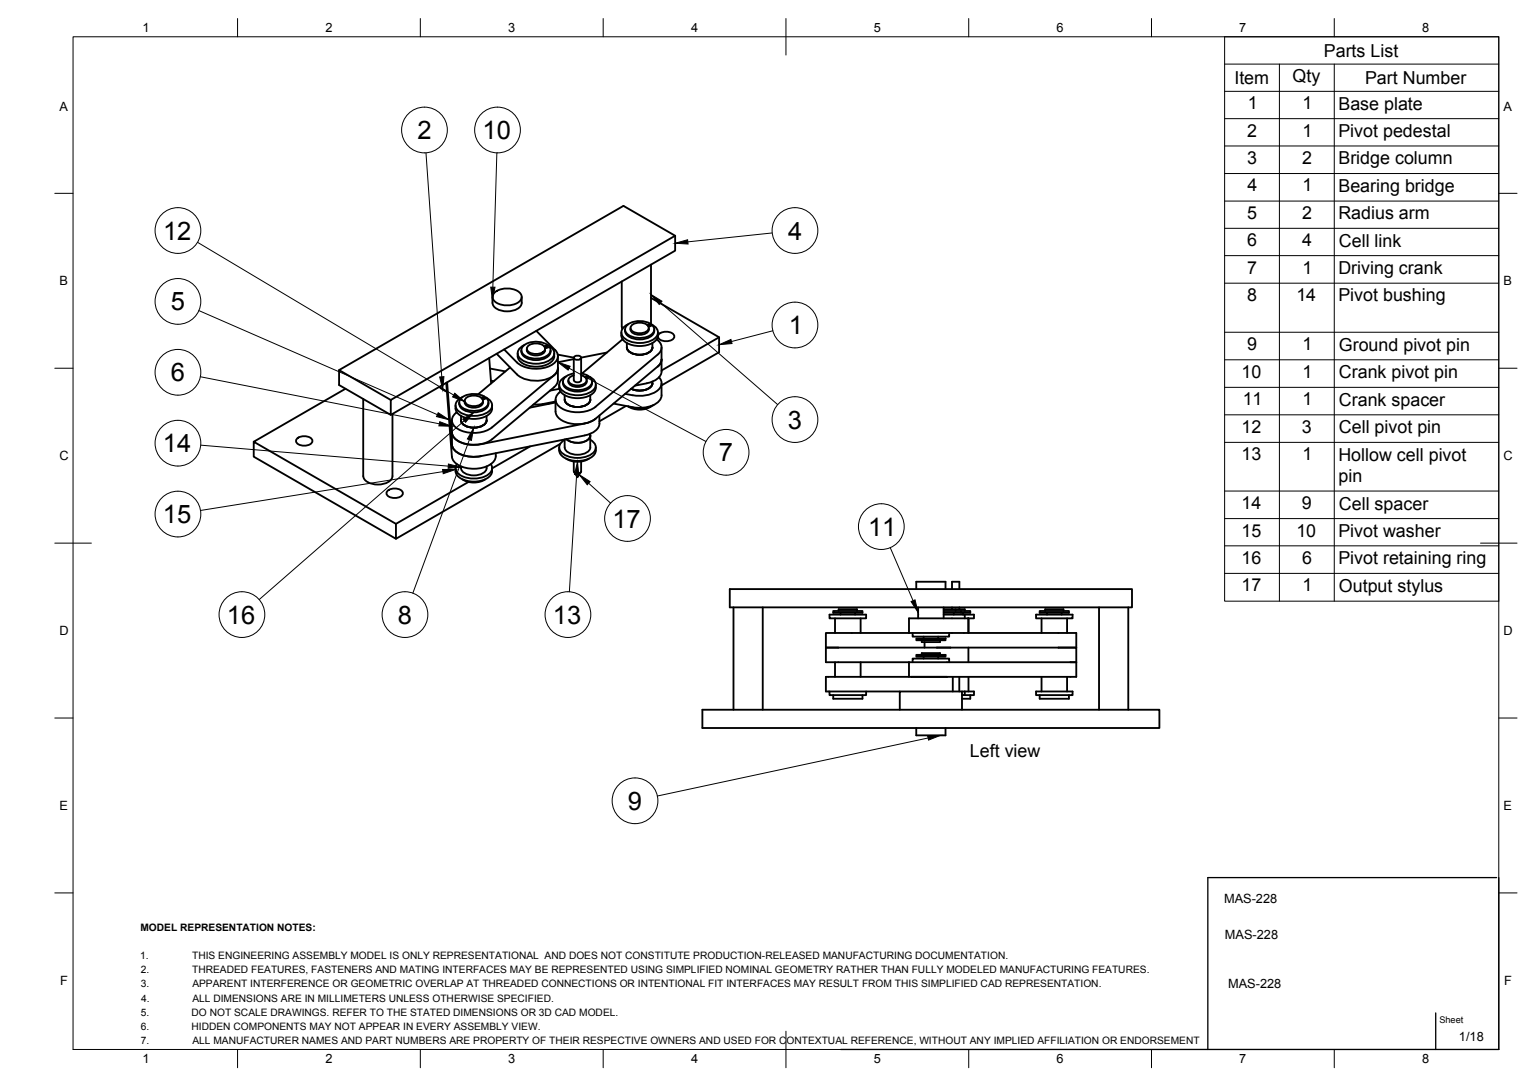
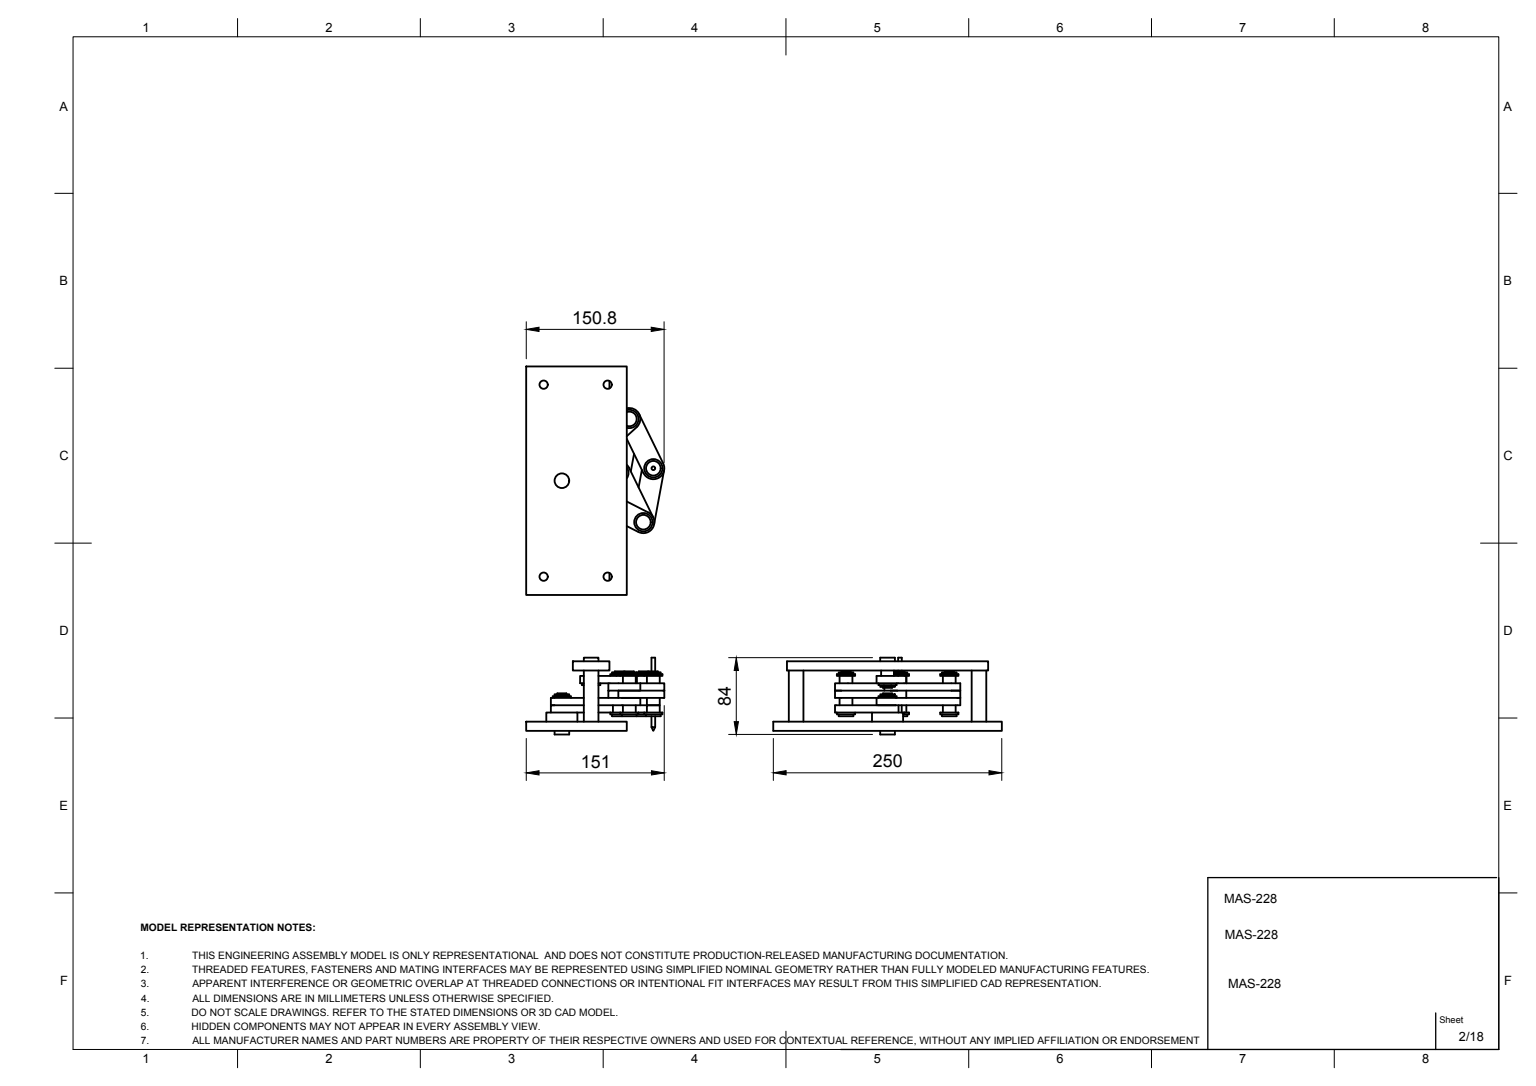
ISO-10303-21;
HEADER;
/* Generated by software containing ST-Developer
 * from STEP Tools, Inc. (www.steptools.com) 
 */

FILE_DESCRIPTION(
/* description */ ('Independent Peaucellier-Lipkin straight-line linkage. Radius arms 100
 mm, inversion-cell links 60 mm, crank radius and fixed-pivot spacing 
32 mm. Inversion constant 6400 mm squared, nominal output straight lin
e X=100 mm. Overhead bearing bridge clears the layered moving links. N
o accuracy or load rating assigned.'),
/* implementation_level */ '2;1');

FILE_NAME(
/* name */ 'MAS-228.step',
/* time_stamp */ '2026-11-09T18:06:16-08:00',
/* author */ (''),
/* organization */ (''),
/* preprocessor_version */ 'ST-DEVELOPER v20.2',
/* originating_system */ 'Autodesk Translation Framework v15.17.0.0',
/* authorisation */ '');

FILE_SCHEMA (('AUTOMOTIVE_DESIGN { 1 0 10303 214 3 1 1 }'));
ENDSEC;

DATA;
#10=MECHANICAL_DESIGN_GEOMETRIC_PRESENTATION_REPRESENTATION('',(#282,#283,
#284,#285,#286,#287,#288,#289,#290,#291,#292,#293,#294,#295,#296,#297,#298),
#3581);
#11=ITEM_DEFINED_TRANSFORMATION($,$,#2074,#2300);
#12=ITEM_DEFINED_TRANSFORMATION($,$,#2096,#2301);
#13=ITEM_DEFINED_TRANSFORMATION($,$,#2132,#2302);
#14=ITEM_DEFINED_TRANSFORMATION($,$,#2105,#2303);
#15=ITEM_DEFINED_TRANSFORMATION($,$,#2138,#2304);
#16=ITEM_DEFINED_TRANSFORMATION($,$,#2155,#2305);
#17=ITEM_DEFINED_TRANSFORMATION($,$,#2115,#2306);
#18=ITEM_DEFINED_TRANSFORMATION($,$,#2238,#2307);
#19=ITEM_DEFINED_TRANSFORMATION($,$,#2132,#2308);
#20=ITEM_DEFINED_TRANSFORMATION($,$,#2138,#2309);
#21=ITEM_DEFINED_TRANSFORMATION($,$,#2155,#2310);
#22=ITEM_DEFINED_TRANSFORMATION($,$,#2155,#2311);
#23=ITEM_DEFINED_TRANSFORMATION($,$,#2155,#2312);
#24=ITEM_DEFINED_TRANSFORMATION($,$,#2172,#2313);
#25=ITEM_DEFINED_TRANSFORMATION($,$,#2190,#2314);
#26=ITEM_DEFINED_TRANSFORMATION($,$,#2208,#2315);
#27=ITEM_DEFINED_TRANSFORMATION($,$,#2253,#2316);
#28=ITEM_DEFINED_TRANSFORMATION($,$,#2217,#2317);
#29=ITEM_DEFINED_TRANSFORMATION($,$,#2271,#2318);
#30=ITEM_DEFINED_TRANSFORMATION($,$,#2280,#2319);
#31=ITEM_DEFINED_TRANSFORMATION($,$,#2238,#2320);
#32=ITEM_DEFINED_TRANSFORMATION($,$,#2238,#2321);
#33=ITEM_DEFINED_TRANSFORMATION($,$,#2238,#2322);
#34=ITEM_DEFINED_TRANSFORMATION($,$,#2238,#2323);
#35=ITEM_DEFINED_TRANSFORMATION($,$,#2238,#2324);
#36=ITEM_DEFINED_TRANSFORMATION($,$,#2238,#2325);
#37=ITEM_DEFINED_TRANSFORMATION($,$,#2238,#2326);
#38=ITEM_DEFINED_TRANSFORMATION($,$,#2238,#2327);
#39=ITEM_DEFINED_TRANSFORMATION($,$,#2238,#2328);
#40=ITEM_DEFINED_TRANSFORMATION($,$,#2238,#2329);
#41=ITEM_DEFINED_TRANSFORMATION($,$,#2238,#2330);
#42=ITEM_DEFINED_TRANSFORMATION($,$,#2238,#2331);
#43=ITEM_DEFINED_TRANSFORMATION($,$,#2238,#2332);
#44=ITEM_DEFINED_TRANSFORMATION($,$,#2289,#2333);
#45=ITEM_DEFINED_TRANSFORMATION($,$,#2247,#2334);
#46=ITEM_DEFINED_TRANSFORMATION($,$,#2280,#2335);
#47=ITEM_DEFINED_TRANSFORMATION($,$,#2289,#2336);
#48=ITEM_DEFINED_TRANSFORMATION($,$,#2271,#2337);
#49=ITEM_DEFINED_TRANSFORMATION($,$,#2280,#2338);
#50=ITEM_DEFINED_TRANSFORMATION($,$,#2280,#2339);
#51=ITEM_DEFINED_TRANSFORMATION($,$,#2289,#2340);
#52=ITEM_DEFINED_TRANSFORMATION($,$,#2253,#2341);
#53=ITEM_DEFINED_TRANSFORMATION($,$,#2271,#2342);
#54=ITEM_DEFINED_TRANSFORMATION($,$,#2271,#2343);
#55=ITEM_DEFINED_TRANSFORMATION($,$,#2280,#2344);
#56=ITEM_DEFINED_TRANSFORMATION($,$,#2280,#2345);
#57=ITEM_DEFINED_TRANSFORMATION($,$,#2289,#2346);
#58=ITEM_DEFINED_TRANSFORMATION($,$,#2253,#2347);
#59=ITEM_DEFINED_TRANSFORMATION($,$,#2271,#2348);
#60=ITEM_DEFINED_TRANSFORMATION($,$,#2271,#2349);
#61=ITEM_DEFINED_TRANSFORMATION($,$,#2280,#2350);
#62=ITEM_DEFINED_TRANSFORMATION($,$,#2280,#2351);
#63=ITEM_DEFINED_TRANSFORMATION($,$,#2289,#2352);
#64=ITEM_DEFINED_TRANSFORMATION($,$,#2271,#2353);
#65=ITEM_DEFINED_TRANSFORMATION($,$,#2271,#2354);
#66=ITEM_DEFINED_TRANSFORMATION($,$,#2271,#2355);
#67=ITEM_DEFINED_TRANSFORMATION($,$,#2280,#2356);
#68=ITEM_DEFINED_TRANSFORMATION($,$,#2280,#2357);
#69=ITEM_DEFINED_TRANSFORMATION($,$,#2289,#2358);
#70=(
REPRESENTATION_RELATIONSHIP($,$,#3682,#3681)
REPRESENTATION_RELATIONSHIP_WITH_TRANSFORMATION(#11)
SHAPE_REPRESENTATION_RELATIONSHIP()
);
#71=(
REPRESENTATION_RELATIONSHIP($,$,#3683,#3681)
REPRESENTATION_RELATIONSHIP_WITH_TRANSFORMATION(#12)
SHAPE_REPRESENTATION_RELATIONSHIP()
);
#72=(
REPRESENTATION_RELATIONSHIP($,$,#3686,#3681)
REPRESENTATION_RELATIONSHIP_WITH_TRANSFORMATION(#13)
SHAPE_REPRESENTATION_RELATIONSHIP()
);
#73=(
REPRESENTATION_RELATIONSHIP($,$,#3684,#3681)
REPRESENTATION_RELATIONSHIP_WITH_TRANSFORMATION(#14)
SHAPE_REPRESENTATION_RELATIONSHIP()
);
#74=(
REPRESENTATION_RELATIONSHIP($,$,#3687,#3681)
REPRESENTATION_RELATIONSHIP_WITH_TRANSFORMATION(#15)
SHAPE_REPRESENTATION_RELATIONSHIP()
);
#75=(
REPRESENTATION_RELATIONSHIP($,$,#3688,#3681)
REPRESENTATION_RELATIONSHIP_WITH_TRANSFORMATION(#16)
SHAPE_REPRESENTATION_RELATIONSHIP()
);
#76=(
REPRESENTATION_RELATIONSHIP($,$,#3685,#3681)
REPRESENTATION_RELATIONSHIP_WITH_TRANSFORMATION(#17)
SHAPE_REPRESENTATION_RELATIONSHIP()
);
#77=(
REPRESENTATION_RELATIONSHIP($,$,#3693,#3681)
REPRESENTATION_RELATIONSHIP_WITH_TRANSFORMATION(#18)
SHAPE_REPRESENTATION_RELATIONSHIP()
);
#78=(
REPRESENTATION_RELATIONSHIP($,$,#3686,#3681)
REPRESENTATION_RELATIONSHIP_WITH_TRANSFORMATION(#19)
SHAPE_REPRESENTATION_RELATIONSHIP()
);
#79=(
REPRESENTATION_RELATIONSHIP($,$,#3687,#3681)
REPRESENTATION_RELATIONSHIP_WITH_TRANSFORMATION(#20)
SHAPE_REPRESENTATION_RELATIONSHIP()
);
#80=(
REPRESENTATION_RELATIONSHIP($,$,#3688,#3681)
REPRESENTATION_RELATIONSHIP_WITH_TRANSFORMATION(#21)
SHAPE_REPRESENTATION_RELATIONSHIP()
);
#81=(
REPRESENTATION_RELATIONSHIP($,$,#3688,#3681)
REPRESENTATION_RELATIONSHIP_WITH_TRANSFORMATION(#22)
SHAPE_REPRESENTATION_RELATIONSHIP()
);
#82=(
REPRESENTATION_RELATIONSHIP($,$,#3688,#3681)
REPRESENTATION_RELATIONSHIP_WITH_TRANSFORMATION(#23)
SHAPE_REPRESENTATION_RELATIONSHIP()
);
#83=(
REPRESENTATION_RELATIONSHIP($,$,#3689,#3681)
REPRESENTATION_RELATIONSHIP_WITH_TRANSFORMATION(#24)
SHAPE_REPRESENTATION_RELATIONSHIP()
);
#84=(
REPRESENTATION_RELATIONSHIP($,$,#3690,#3681)
REPRESENTATION_RELATIONSHIP_WITH_TRANSFORMATION(#25)
SHAPE_REPRESENTATION_RELATIONSHIP()
);
#85=(
REPRESENTATION_RELATIONSHIP($,$,#3691,#3681)
REPRESENTATION_RELATIONSHIP_WITH_TRANSFORMATION(#26)
SHAPE_REPRESENTATION_RELATIONSHIP()
);
#86=(
REPRESENTATION_RELATIONSHIP($,$,#3695,#3681)
REPRESENTATION_RELATIONSHIP_WITH_TRANSFORMATION(#27)
SHAPE_REPRESENTATION_RELATIONSHIP()
);
#87=(
REPRESENTATION_RELATIONSHIP($,$,#3692,#3681)
REPRESENTATION_RELATIONSHIP_WITH_TRANSFORMATION(#28)
SHAPE_REPRESENTATION_RELATIONSHIP()
);
#88=(
REPRESENTATION_RELATIONSHIP($,$,#3696,#3681)
REPRESENTATION_RELATIONSHIP_WITH_TRANSFORMATION(#29)
SHAPE_REPRESENTATION_RELATIONSHIP()
);
#89=(
REPRESENTATION_RELATIONSHIP($,$,#3697,#3681)
REPRESENTATION_RELATIONSHIP_WITH_TRANSFORMATION(#30)
SHAPE_REPRESENTATION_RELATIONSHIP()
);
#90=(
REPRESENTATION_RELATIONSHIP($,$,#3693,#3681)
REPRESENTATION_RELATIONSHIP_WITH_TRANSFORMATION(#31)
SHAPE_REPRESENTATION_RELATIONSHIP()
);
#91=(
REPRESENTATION_RELATIONSHIP($,$,#3693,#3681)
REPRESENTATION_RELATIONSHIP_WITH_TRANSFORMATION(#32)
SHAPE_REPRESENTATION_RELATIONSHIP()
);
#92=(
REPRESENTATION_RELATIONSHIP($,$,#3693,#3681)
REPRESENTATION_RELATIONSHIP_WITH_TRANSFORMATION(#33)
SHAPE_REPRESENTATION_RELATIONSHIP()
);
#93=(
REPRESENTATION_RELATIONSHIP($,$,#3693,#3681)
REPRESENTATION_RELATIONSHIP_WITH_TRANSFORMATION(#34)
SHAPE_REPRESENTATION_RELATIONSHIP()
);
#94=(
REPRESENTATION_RELATIONSHIP($,$,#3693,#3681)
REPRESENTATION_RELATIONSHIP_WITH_TRANSFORMATION(#35)
SHAPE_REPRESENTATION_RELATIONSHIP()
);
#95=(
REPRESENTATION_RELATIONSHIP($,$,#3693,#3681)
REPRESENTATION_RELATIONSHIP_WITH_TRANSFORMATION(#36)
SHAPE_REPRESENTATION_RELATIONSHIP()
);
#96=(
REPRESENTATION_RELATIONSHIP($,$,#3693,#3681)
REPRESENTATION_RELATIONSHIP_WITH_TRANSFORMATION(#37)
SHAPE_REPRESENTATION_RELATIONSHIP()
);
#97=(
REPRESENTATION_RELATIONSHIP($,$,#3693,#3681)
REPRESENTATION_RELATIONSHIP_WITH_TRANSFORMATION(#38)
SHAPE_REPRESENTATION_RELATIONSHIP()
);
#98=(
REPRESENTATION_RELATIONSHIP($,$,#3693,#3681)
REPRESENTATION_RELATIONSHIP_WITH_TRANSFORMATION(#39)
SHAPE_REPRESENTATION_RELATIONSHIP()
);
#99=(
REPRESENTATION_RELATIONSHIP($,$,#3693,#3681)
REPRESENTATION_RELATIONSHIP_WITH_TRANSFORMATION(#40)
SHAPE_REPRESENTATION_RELATIONSHIP()
);
#100=(
REPRESENTATION_RELATIONSHIP($,$,#3693,#3681)
REPRESENTATION_RELATIONSHIP_WITH_TRANSFORMATION(#41)
SHAPE_REPRESENTATION_RELATIONSHIP()
);
#101=(
REPRESENTATION_RELATIONSHIP($,$,#3693,#3681)
REPRESENTATION_RELATIONSHIP_WITH_TRANSFORMATION(#42)
SHAPE_REPRESENTATION_RELATIONSHIP()
);
#102=(
REPRESENTATION_RELATIONSHIP($,$,#3693,#3681)
REPRESENTATION_RELATIONSHIP_WITH_TRANSFORMATION(#43)
SHAPE_REPRESENTATION_RELATIONSHIP()
);
#103=(
REPRESENTATION_RELATIONSHIP($,$,#3698,#3681)
REPRESENTATION_RELATIONSHIP_WITH_TRANSFORMATION(#44)
SHAPE_REPRESENTATION_RELATIONSHIP()
);
#104=(
REPRESENTATION_RELATIONSHIP($,$,#3694,#3681)
REPRESENTATION_RELATIONSHIP_WITH_TRANSFORMATION(#45)
SHAPE_REPRESENTATION_RELATIONSHIP()
);
#105=(
REPRESENTATION_RELATIONSHIP($,$,#3697,#3681)
REPRESENTATION_RELATIONSHIP_WITH_TRANSFORMATION(#46)
SHAPE_REPRESENTATION_RELATIONSHIP()
);
#106=(
REPRESENTATION_RELATIONSHIP($,$,#3698,#3681)
REPRESENTATION_RELATIONSHIP_WITH_TRANSFORMATION(#47)
SHAPE_REPRESENTATION_RELATIONSHIP()
);
#107=(
REPRESENTATION_RELATIONSHIP($,$,#3696,#3681)
REPRESENTATION_RELATIONSHIP_WITH_TRANSFORMATION(#48)
SHAPE_REPRESENTATION_RELATIONSHIP()
);
#108=(
REPRESENTATION_RELATIONSHIP($,$,#3697,#3681)
REPRESENTATION_RELATIONSHIP_WITH_TRANSFORMATION(#49)
SHAPE_REPRESENTATION_RELATIONSHIP()
);
#109=(
REPRESENTATION_RELATIONSHIP($,$,#3697,#3681)
REPRESENTATION_RELATIONSHIP_WITH_TRANSFORMATION(#50)
SHAPE_REPRESENTATION_RELATIONSHIP()
);
#110=(
REPRESENTATION_RELATIONSHIP($,$,#3698,#3681)
REPRESENTATION_RELATIONSHIP_WITH_TRANSFORMATION(#51)
SHAPE_REPRESENTATION_RELATIONSHIP()
);
#111=(
REPRESENTATION_RELATIONSHIP($,$,#3695,#3681)
REPRESENTATION_RELATIONSHIP_WITH_TRANSFORMATION(#52)
SHAPE_REPRESENTATION_RELATIONSHIP()
);
#112=(
REPRESENTATION_RELATIONSHIP($,$,#3696,#3681)
REPRESENTATION_RELATIONSHIP_WITH_TRANSFORMATION(#53)
SHAPE_REPRESENTATION_RELATIONSHIP()
);
#113=(
REPRESENTATION_RELATIONSHIP($,$,#3696,#3681)
REPRESENTATION_RELATIONSHIP_WITH_TRANSFORMATION(#54)
SHAPE_REPRESENTATION_RELATIONSHIP()
);
#114=(
REPRESENTATION_RELATIONSHIP($,$,#3697,#3681)
REPRESENTATION_RELATIONSHIP_WITH_TRANSFORMATION(#55)
SHAPE_REPRESENTATION_RELATIONSHIP()
);
#115=(
REPRESENTATION_RELATIONSHIP($,$,#3697,#3681)
REPRESENTATION_RELATIONSHIP_WITH_TRANSFORMATION(#56)
SHAPE_REPRESENTATION_RELATIONSHIP()
);
#116=(
REPRESENTATION_RELATIONSHIP($,$,#3698,#3681)
REPRESENTATION_RELATIONSHIP_WITH_TRANSFORMATION(#57)
SHAPE_REPRESENTATION_RELATIONSHIP()
);
#117=(
REPRESENTATION_RELATIONSHIP($,$,#3695,#3681)
REPRESENTATION_RELATIONSHIP_WITH_TRANSFORMATION(#58)
SHAPE_REPRESENTATION_RELATIONSHIP()
);
#118=(
REPRESENTATION_RELATIONSHIP($,$,#3696,#3681)
REPRESENTATION_RELATIONSHIP_WITH_TRANSFORMATION(#59)
SHAPE_REPRESENTATION_RELATIONSHIP()
);
#119=(
REPRESENTATION_RELATIONSHIP($,$,#3696,#3681)
REPRESENTATION_RELATIONSHIP_WITH_TRANSFORMATION(#60)
SHAPE_REPRESENTATION_RELATIONSHIP()
);
#120=(
REPRESENTATION_RELATIONSHIP($,$,#3697,#3681)
REPRESENTATION_RELATIONSHIP_WITH_TRANSFORMATION(#61)
SHAPE_REPRESENTATION_RELATIONSHIP()
);
#121=(
REPRESENTATION_RELATIONSHIP($,$,#3697,#3681)
REPRESENTATION_RELATIONSHIP_WITH_TRANSFORMATION(#62)
SHAPE_REPRESENTATION_RELATIONSHIP()
);
#122=(
REPRESENTATION_RELATIONSHIP($,$,#3698,#3681)
REPRESENTATION_RELATIONSHIP_WITH_TRANSFORMATION(#63)
SHAPE_REPRESENTATION_RELATIONSHIP()
);
#123=(
REPRESENTATION_RELATIONSHIP($,$,#3696,#3681)
REPRESENTATION_RELATIONSHIP_WITH_TRANSFORMATION(#64)
SHAPE_REPRESENTATION_RELATIONSHIP()
);
#124=(
REPRESENTATION_RELATIONSHIP($,$,#3696,#3681)
REPRESENTATION_RELATIONSHIP_WITH_TRANSFORMATION(#65)
SHAPE_REPRESENTATION_RELATIONSHIP()
);
#125=(
REPRESENTATION_RELATIONSHIP($,$,#3696,#3681)
REPRESENTATION_RELATIONSHIP_WITH_TRANSFORMATION(#66)
SHAPE_REPRESENTATION_RELATIONSHIP()
);
#126=(
REPRESENTATION_RELATIONSHIP($,$,#3697,#3681)
REPRESENTATION_RELATIONSHIP_WITH_TRANSFORMATION(#67)
SHAPE_REPRESENTATION_RELATIONSHIP()
);
#127=(
REPRESENTATION_RELATIONSHIP($,$,#3697,#3681)
REPRESENTATION_RELATIONSHIP_WITH_TRANSFORMATION(#68)
SHAPE_REPRESENTATION_RELATIONSHIP()
);
#128=(
REPRESENTATION_RELATIONSHIP($,$,#3698,#3681)
REPRESENTATION_RELATIONSHIP_WITH_TRANSFORMATION(#69)
SHAPE_REPRESENTATION_RELATIONSHIP()
);
#129=CONTEXT_DEPENDENT_SHAPE_REPRESENTATION(#70,#3622);
#130=CONTEXT_DEPENDENT_SHAPE_REPRESENTATION(#71,#3623);
#131=CONTEXT_DEPENDENT_SHAPE_REPRESENTATION(#72,#3624);
#132=CONTEXT_DEPENDENT_SHAPE_REPRESENTATION(#73,#3625);
#133=CONTEXT_DEPENDENT_SHAPE_REPRESENTATION(#74,#3626);
#134=CONTEXT_DEPENDENT_SHAPE_REPRESENTATION(#75,#3627);
#135=CONTEXT_DEPENDENT_SHAPE_REPRESENTATION(#76,#3628);
#136=CONTEXT_DEPENDENT_SHAPE_REPRESENTATION(#77,#3629);
#137=CONTEXT_DEPENDENT_SHAPE_REPRESENTATION(#78,#3630);
#138=CONTEXT_DEPENDENT_SHAPE_REPRESENTATION(#79,#3631);
#139=CONTEXT_DEPENDENT_SHAPE_REPRESENTATION(#80,#3632);
#140=CONTEXT_DEPENDENT_SHAPE_REPRESENTATION(#81,#3633);
#141=CONTEXT_DEPENDENT_SHAPE_REPRESENTATION(#82,#3634);
#142=CONTEXT_DEPENDENT_SHAPE_REPRESENTATION(#83,#3635);
#143=CONTEXT_DEPENDENT_SHAPE_REPRESENTATION(#84,#3636);
#144=CONTEXT_DEPENDENT_SHAPE_REPRESENTATION(#85,#3637);
#145=CONTEXT_DEPENDENT_SHAPE_REPRESENTATION(#86,#3638);
#146=CONTEXT_DEPENDENT_SHAPE_REPRESENTATION(#87,#3639);
#147=CONTEXT_DEPENDENT_SHAPE_REPRESENTATION(#88,#3640);
#148=CONTEXT_DEPENDENT_SHAPE_REPRESENTATION(#89,#3641);
#149=CONTEXT_DEPENDENT_SHAPE_REPRESENTATION(#90,#3642);
#150=CONTEXT_DEPENDENT_SHAPE_REPRESENTATION(#91,#3643);
#151=CONTEXT_DEPENDENT_SHAPE_REPRESENTATION(#92,#3644);
#152=CONTEXT_DEPENDENT_SHAPE_REPRESENTATION(#93,#3645);
#153=CONTEXT_DEPENDENT_SHAPE_REPRESENTATION(#94,#3646);
#154=CONTEXT_DEPENDENT_SHAPE_REPRESENTATION(#95,#3647);
#155=CONTEXT_DEPENDENT_SHAPE_REPRESENTATION(#96,#3648);
#156=CONTEXT_DEPENDENT_SHAPE_REPRESENTATION(#97,#3649);
#157=CONTEXT_DEPENDENT_SHAPE_REPRESENTATION(#98,#3650);
#158=CONTEXT_DEPENDENT_SHAPE_REPRESENTATION(#99,#3651);
#159=CONTEXT_DEPENDENT_SHAPE_REPRESENTATION(#100,#3652);
#160=CONTEXT_DEPENDENT_SHAPE_REPRESENTATION(#101,#3653);
#161=CONTEXT_DEPENDENT_SHAPE_REPRESENTATION(#102,#3654);
#162=CONTEXT_DEPENDENT_SHAPE_REPRESENTATION(#103,#3655);
#163=CONTEXT_DEPENDENT_SHAPE_REPRESENTATION(#104,#3656);
#164=CONTEXT_DEPENDENT_SHAPE_REPRESENTATION(#105,#3657);
#165=CONTEXT_DEPENDENT_SHAPE_REPRESENTATION(#106,#3658);
#166=CONTEXT_DEPENDENT_SHAPE_REPRESENTATION(#107,#3659);
#167=CONTEXT_DEPENDENT_SHAPE_REPRESENTATION(#108,#3660);
#168=CONTEXT_DEPENDENT_SHAPE_REPRESENTATION(#109,#3661);
#169=CONTEXT_DEPENDENT_SHAPE_REPRESENTATION(#110,#3662);
#170=CONTEXT_DEPENDENT_SHAPE_REPRESENTATION(#111,#3663);
#171=CONTEXT_DEPENDENT_SHAPE_REPRESENTATION(#112,#3664);
#172=CONTEXT_DEPENDENT_SHAPE_REPRESENTATION(#113,#3665);
#173=CONTEXT_DEPENDENT_SHAPE_REPRESENTATION(#114,#3666);
#174=CONTEXT_DEPENDENT_SHAPE_REPRESENTATION(#115,#3667);
#175=CONTEXT_DEPENDENT_SHAPE_REPRESENTATION(#116,#3668);
#176=CONTEXT_DEPENDENT_SHAPE_REPRESENTATION(#117,#3669);
#177=CONTEXT_DEPENDENT_SHAPE_REPRESENTATION(#118,#3670);
#178=CONTEXT_DEPENDENT_SHAPE_REPRESENTATION(#119,#3671);
#179=CONTEXT_DEPENDENT_SHAPE_REPRESENTATION(#120,#3672);
#180=CONTEXT_DEPENDENT_SHAPE_REPRESENTATION(#121,#3673);
#181=CONTEXT_DEPENDENT_SHAPE_REPRESENTATION(#122,#3674);
#182=CONTEXT_DEPENDENT_SHAPE_REPRESENTATION(#123,#3675);
#183=CONTEXT_DEPENDENT_SHAPE_REPRESENTATION(#124,#3676);
#184=CONTEXT_DEPENDENT_SHAPE_REPRESENTATION(#125,#3677);
#185=CONTEXT_DEPENDENT_SHAPE_REPRESENTATION(#126,#3678);
#186=CONTEXT_DEPENDENT_SHAPE_REPRESENTATION(#127,#3679);
#187=CONTEXT_DEPENDENT_SHAPE_REPRESENTATION(#128,#3680);
#188=NEXT_ASSEMBLY_USAGE_OCCURRENCE('Base plate:1','Base plate:1',
'Base plate:1',#3700,#3701,'Base plate:1');
#189=NEXT_ASSEMBLY_USAGE_OCCURRENCE('Pivot pedestal:1',
'Pivot pedestal:1','Pivot pedestal:1',#3700,#3702,'Pivot pedestal:1');
#190=NEXT_ASSEMBLY_USAGE_OCCURRENCE('Bridge column:1','Bridge column:1',
'Bridge column:1',#3700,#3705,'Bridge column:1');
#191=NEXT_ASSEMBLY_USAGE_OCCURRENCE('Bearing bridge:1',
'Bearing bridge:1','Bearing bridge:1',#3700,#3703,'Bearing bridge:1');
#192=NEXT_ASSEMBLY_USAGE_OCCURRENCE('Radius arm:1','Radius arm:1',
'Radius arm:1',#3700,#3706,'Radius arm:1');
#193=NEXT_ASSEMBLY_USAGE_OCCURRENCE('Cell link:1','Cell link:1',
'Cell link:1',#3700,#3707,'Cell link:1');
#194=NEXT_ASSEMBLY_USAGE_OCCURRENCE('Driving crank:1','Driving crank:1',
'Driving crank:1',#3700,#3704,'Driving crank:1');
#195=NEXT_ASSEMBLY_USAGE_OCCURRENCE('Pivot bushing:1','Pivot bushing:1',
'Pivot bushing:1',#3700,#3712,'Pivot bushing:1');
#196=NEXT_ASSEMBLY_USAGE_OCCURRENCE('Bridge column:2','Bridge column:2',
'Bridge column:2',#3700,#3705,'Bridge column:2');
#197=NEXT_ASSEMBLY_USAGE_OCCURRENCE('Radius arm:2','Radius arm:2',
'Radius arm:2',#3700,#3706,'Radius arm:2');
#198=NEXT_ASSEMBLY_USAGE_OCCURRENCE('Cell link:2','Cell link:2',
'Cell link:2',#3700,#3707,'Cell link:2');
#199=NEXT_ASSEMBLY_USAGE_OCCURRENCE('Cell link:3','Cell link:3',
'Cell link:3',#3700,#3707,'Cell link:3');
#200=NEXT_ASSEMBLY_USAGE_OCCURRENCE('Cell link:4','Cell link:4',
'Cell link:4',#3700,#3707,'Cell link:4');
#201=NEXT_ASSEMBLY_USAGE_OCCURRENCE('Ground pivot pin:1',
'Ground pivot pin:1','Ground pivot pin:1',#3700,#3708,
'Ground pivot pin:1');
#202=NEXT_ASSEMBLY_USAGE_OCCURRENCE('Crank pivot pin:1',
'Crank pivot pin:1','Crank pivot pin:1',#3700,#3709,'Crank pivot pin:1');
#203=NEXT_ASSEMBLY_USAGE_OCCURRENCE('Crank spacer:1','Crank spacer:1',
'Crank spacer:1',#3700,#3710,'Crank spacer:1');
#204=NEXT_ASSEMBLY_USAGE_OCCURRENCE('Cell pivot pin:1',
'Cell pivot pin:1','Cell pivot pin:1',#3700,#3714,'Cell pivot pin:1');
#205=NEXT_ASSEMBLY_USAGE_OCCURRENCE('Hollow cell pivot pin:1',
'Hollow cell pivot pin:1','Hollow cell pivot pin:1',#3700,#3711,
'Hollow cell pivot pin:1');
#206=NEXT_ASSEMBLY_USAGE_OCCURRENCE('Cell spacer:1','Cell spacer:1',
'Cell spacer:1',#3700,#3715,'Cell spacer:1');
#207=NEXT_ASSEMBLY_USAGE_OCCURRENCE('Pivot washer:1','Pivot washer:1',
'Pivot washer:1',#3700,#3716,'Pivot washer:1');
#208=NEXT_ASSEMBLY_USAGE_OCCURRENCE('Pivot bushing:2','Pivot bushing:2',
'Pivot bushing:2',#3700,#3712,'Pivot bushing:2');
#209=NEXT_ASSEMBLY_USAGE_OCCURRENCE('Pivot bushing:3','Pivot bushing:3',
'Pivot bushing:3',#3700,#3712,'Pivot bushing:3');
#210=NEXT_ASSEMBLY_USAGE_OCCURRENCE('Pivot bushing:4','Pivot bushing:4',
'Pivot bushing:4',#3700,#3712,'Pivot bushing:4');
#211=NEXT_ASSEMBLY_USAGE_OCCURRENCE('Pivot bushing:5','Pivot bushing:5',
'Pivot bushing:5',#3700,#3712,'Pivot bushing:5');
#212=NEXT_ASSEMBLY_USAGE_OCCURRENCE('Pivot bushing:6','Pivot bushing:6',
'Pivot bushing:6',#3700,#3712,'Pivot bushing:6');
#213=NEXT_ASSEMBLY_USAGE_OCCURRENCE('Pivot bushing:7','Pivot bushing:7',
'Pivot bushing:7',#3700,#3712,'Pivot bushing:7');
#214=NEXT_ASSEMBLY_USAGE_OCCURRENCE('Pivot bushing:8','Pivot bushing:8',
'Pivot bushing:8',#3700,#3712,'Pivot bushing:8');
#215=NEXT_ASSEMBLY_USAGE_OCCURRENCE('Pivot bushing:9','Pivot bushing:9',
'Pivot bushing:9',#3700,#3712,'Pivot bushing:9');
#216=NEXT_ASSEMBLY_USAGE_OCCURRENCE('Pivot bushing:10',
'Pivot bushing:10','Pivot bushing:10',#3700,#3712,'Pivot bushing:10');
#217=NEXT_ASSEMBLY_USAGE_OCCURRENCE('Pivot bushing:11',
'Pivot bushing:11','Pivot bushing:11',#3700,#3712,'Pivot bushing:11');
#218=NEXT_ASSEMBLY_USAGE_OCCURRENCE('Pivot bushing:12',
'Pivot bushing:12','Pivot bushing:12',#3700,#3712,'Pivot bushing:12');
#219=NEXT_ASSEMBLY_USAGE_OCCURRENCE('Pivot bushing:13',
'Pivot bushing:13','Pivot bushing:13',#3700,#3712,'Pivot bushing:13');
#220=NEXT_ASSEMBLY_USAGE_OCCURRENCE('Pivot bushing:14',
'Pivot bushing:14','Pivot bushing:14',#3700,#3712,'Pivot bushing:14');
#221=NEXT_ASSEMBLY_USAGE_OCCURRENCE('Pivot retaining ring:1',
'Pivot retaining ring:1','Pivot retaining ring:1',#3700,#3717,
'Pivot retaining ring:1');
#222=NEXT_ASSEMBLY_USAGE_OCCURRENCE('Output stylus:1','Output stylus:1',
'Output stylus:1',#3700,#3713,'Output stylus:1');
#223=NEXT_ASSEMBLY_USAGE_OCCURRENCE('Pivot washer:2','Pivot washer:2',
'Pivot washer:2',#3700,#3716,'Pivot washer:2');
#224=NEXT_ASSEMBLY_USAGE_OCCURRENCE('Pivot retaining ring:2',
'Pivot retaining ring:2','Pivot retaining ring:2',#3700,#3717,
'Pivot retaining ring:2');
#225=NEXT_ASSEMBLY_USAGE_OCCURRENCE('Cell spacer:2','Cell spacer:2',
'Cell spacer:2',#3700,#3715,'Cell spacer:2');
#226=NEXT_ASSEMBLY_USAGE_OCCURRENCE('Pivot washer:3','Pivot washer:3',
'Pivot washer:3',#3700,#3716,'Pivot washer:3');
#227=NEXT_ASSEMBLY_USAGE_OCCURRENCE('Pivot washer:4','Pivot washer:4',
'Pivot washer:4',#3700,#3716,'Pivot washer:4');
#228=NEXT_ASSEMBLY_USAGE_OCCURRENCE('Pivot retaining ring:3',
'Pivot retaining ring:3','Pivot retaining ring:3',#3700,#3717,
'Pivot retaining ring:3');
#229=NEXT_ASSEMBLY_USAGE_OCCURRENCE('Cell pivot pin:2',
'Cell pivot pin:2','Cell pivot pin:2',#3700,#3714,'Cell pivot pin:2');
#230=NEXT_ASSEMBLY_USAGE_OCCURRENCE('Cell spacer:3','Cell spacer:3',
'Cell spacer:3',#3700,#3715,'Cell spacer:3');
#231=NEXT_ASSEMBLY_USAGE_OCCURRENCE('Cell spacer:4','Cell spacer:4',
'Cell spacer:4',#3700,#3715,'Cell spacer:4');
#232=NEXT_ASSEMBLY_USAGE_OCCURRENCE('Pivot washer:5','Pivot washer:5',
'Pivot washer:5',#3700,#3716,'Pivot washer:5');
#233=NEXT_ASSEMBLY_USAGE_OCCURRENCE('Pivot washer:6','Pivot washer:6',
'Pivot washer:6',#3700,#3716,'Pivot washer:6');
#234=NEXT_ASSEMBLY_USAGE_OCCURRENCE('Pivot retaining ring:4',
'Pivot retaining ring:4','Pivot retaining ring:4',#3700,#3717,
'Pivot retaining ring:4');
#235=NEXT_ASSEMBLY_USAGE_OCCURRENCE('Cell pivot pin:3',
'Cell pivot pin:3','Cell pivot pin:3',#3700,#3714,'Cell pivot pin:3');
#236=NEXT_ASSEMBLY_USAGE_OCCURRENCE('Cell spacer:5','Cell spacer:5',
'Cell spacer:5',#3700,#3715,'Cell spacer:5');
#237=NEXT_ASSEMBLY_USAGE_OCCURRENCE('Cell spacer:6','Cell spacer:6',
'Cell spacer:6',#3700,#3715,'Cell spacer:6');
#238=NEXT_ASSEMBLY_USAGE_OCCURRENCE('Pivot washer:7','Pivot washer:7',
'Pivot washer:7',#3700,#3716,'Pivot washer:7');
#239=NEXT_ASSEMBLY_USAGE_OCCURRENCE('Pivot washer:8','Pivot washer:8',
'Pivot washer:8',#3700,#3716,'Pivot washer:8');
#240=NEXT_ASSEMBLY_USAGE_OCCURRENCE('Pivot retaining ring:5',
'Pivot retaining ring:5','Pivot retaining ring:5',#3700,#3717,
'Pivot retaining ring:5');
#241=NEXT_ASSEMBLY_USAGE_OCCURRENCE('Cell spacer:7','Cell spacer:7',
'Cell spacer:7',#3700,#3715,'Cell spacer:7');
#242=NEXT_ASSEMBLY_USAGE_OCCURRENCE('Cell spacer:8','Cell spacer:8',
'Cell spacer:8',#3700,#3715,'Cell spacer:8');
#243=NEXT_ASSEMBLY_USAGE_OCCURRENCE('Cell spacer:9','Cell spacer:9',
'Cell spacer:9',#3700,#3715,'Cell spacer:9');
#244=NEXT_ASSEMBLY_USAGE_OCCURRENCE('Pivot washer:9','Pivot washer:9',
'Pivot washer:9',#3700,#3716,'Pivot washer:9');
#245=NEXT_ASSEMBLY_USAGE_OCCURRENCE('Pivot washer:10','Pivot washer:10',
'Pivot washer:10',#3700,#3716,'Pivot washer:10');
#246=NEXT_ASSEMBLY_USAGE_OCCURRENCE('Pivot retaining ring:6',
'Pivot retaining ring:6','Pivot retaining ring:6',#3700,#3717,
'Pivot retaining ring:6');
#247=CONICAL_SURFACE('',#2252,1.,0.463647609000806);
#248=SHAPE_REPRESENTATION_RELATIONSHIP('SRR','None',#3682,#265);
#249=SHAPE_REPRESENTATION_RELATIONSHIP('SRR','None',#3683,#266);
#250=SHAPE_REPRESENTATION_RELATIONSHIP('SRR','None',#3684,#267);
#251=SHAPE_REPRESENTATION_RELATIONSHIP('SRR','None',#3685,#268);
#252=SHAPE_REPRESENTATION_RELATIONSHIP('SRR','None',#3686,#269);
#253=SHAPE_REPRESENTATION_RELATIONSHIP('SRR','None',#3687,#270);
#254=SHAPE_REPRESENTATION_RELATIONSHIP('SRR','None',#3688,#271);
#255=SHAPE_REPRESENTATION_RELATIONSHIP('SRR','None',#3689,#272);
#256=SHAPE_REPRESENTATION_RELATIONSHIP('SRR','None',#3690,#273);
#257=SHAPE_REPRESENTATION_RELATIONSHIP('SRR','None',#3691,#274);
#258=SHAPE_REPRESENTATION_RELATIONSHIP('SRR','None',#3692,#275);
#259=SHAPE_REPRESENTATION_RELATIONSHIP('SRR','None',#3693,#276);
#260=SHAPE_REPRESENTATION_RELATIONSHIP('SRR','None',#3694,#277);
#261=SHAPE_REPRESENTATION_RELATIONSHIP('SRR','None',#3695,#278);
#262=SHAPE_REPRESENTATION_RELATIONSHIP('SRR','None',#3696,#279);
#263=SHAPE_REPRESENTATION_RELATIONSHIP('SRR','None',#3697,#280);
#264=SHAPE_REPRESENTATION_RELATIONSHIP('SRR','None',#3698,#281);
#265=ADVANCED_BREP_SHAPE_REPRESENTATION('',(#299),#3564);
#266=ADVANCED_BREP_SHAPE_REPRESENTATION('',(#300),#3565);
#267=ADVANCED_BREP_SHAPE_REPRESENTATION('',(#301),#3566);
#268=ADVANCED_BREP_SHAPE_REPRESENTATION('',(#302),#3567);
#269=ADVANCED_BREP_SHAPE_REPRESENTATION('',(#303),#3568);
#270=ADVANCED_BREP_SHAPE_REPRESENTATION('',(#304),#3569);
#271=ADVANCED_BREP_SHAPE_REPRESENTATION('',(#305),#3570);
#272=ADVANCED_BREP_SHAPE_REPRESENTATION('',(#306),#3571);
#273=ADVANCED_BREP_SHAPE_REPRESENTATION('',(#307),#3572);
#274=ADVANCED_BREP_SHAPE_REPRESENTATION('',(#308),#3573);
#275=ADVANCED_BREP_SHAPE_REPRESENTATION('',(#309),#3574);
#276=ADVANCED_BREP_SHAPE_REPRESENTATION('',(#310),#3575);
#277=ADVANCED_BREP_SHAPE_REPRESENTATION('',(#311),#3576);
#278=ADVANCED_BREP_SHAPE_REPRESENTATION('',(#312),#3577);
#279=ADVANCED_BREP_SHAPE_REPRESENTATION('',(#313),#3578);
#280=ADVANCED_BREP_SHAPE_REPRESENTATION('',(#314),#3579);
#281=ADVANCED_BREP_SHAPE_REPRESENTATION('',(#315),#3580);
#282=STYLED_ITEM('',(#3776),#299);
#283=STYLED_ITEM('',(#3777),#300);
#284=STYLED_ITEM('',(#3778),#301);
#285=STYLED_ITEM('',(#3779),#302);
#286=STYLED_ITEM('',(#3777),#303);
#287=STYLED_ITEM('',(#3780),#304);
#288=STYLED_ITEM('',(#3781),#305);
#289=STYLED_ITEM('',(#3782),#306);
#290=STYLED_ITEM('',(#3782),#307);
#291=STYLED_ITEM('',(#3783),#308);
#292=STYLED_ITEM('',(#3782),#309);
#293=STYLED_ITEM('',(#3784),#310);
#294=STYLED_ITEM('',(#3785),#311);
#295=STYLED_ITEM('',(#3782),#312);
#296=STYLED_ITEM('',(#3783),#313);
#297=STYLED_ITEM('',(#3786),#314);
#298=STYLED_ITEM('',(#3787),#315);
#299=MANIFOLD_SOLID_BREP('Body1',#1868);
#300=MANIFOLD_SOLID_BREP('Body1',#1869);
#301=MANIFOLD_SOLID_BREP('Body1',#1870);
#302=MANIFOLD_SOLID_BREP('Body1',#1871);
#303=MANIFOLD_SOLID_BREP('Body1',#1872);
#304=MANIFOLD_SOLID_BREP('Body1',#1873);
#305=MANIFOLD_SOLID_BREP('Body1',#1874);
#306=MANIFOLD_SOLID_BREP('Body1',#1875);
#307=MANIFOLD_SOLID_BREP('Body1',#1876);
#308=MANIFOLD_SOLID_BREP('Body1',#1877);
#309=MANIFOLD_SOLID_BREP('Body1',#1878);
#310=MANIFOLD_SOLID_BREP('Body1',#1879);
#311=MANIFOLD_SOLID_BREP('Body1',#1880);
#312=MANIFOLD_SOLID_BREP('Body1',#1881);
#313=MANIFOLD_SOLID_BREP('Body1',#1882);
#314=MANIFOLD_SOLID_BREP('Body1',#1883);
#315=MANIFOLD_SOLID_BREP('Body1',#1884);
#316=FACE_BOUND('',#546,.T.);
#317=FACE_BOUND('',#547,.T.);
#318=FACE_BOUND('',#548,.T.);
#319=FACE_BOUND('',#549,.T.);
#320=FACE_BOUND('',#550,.T.);
#321=FACE_BOUND('',#552,.T.);
#322=FACE_BOUND('',#553,.T.);
#323=FACE_BOUND('',#554,.T.);
#324=FACE_BOUND('',#555,.T.);
#325=FACE_BOUND('',#556,.T.);
#326=FACE_BOUND('',#560,.T.);
#327=FACE_BOUND('',#562,.T.);
#328=FACE_BOUND('',#569,.T.);
#329=FACE_BOUND('',#571,.T.);
#330=FACE_BOUND('',#579,.T.);
#331=FACE_BOUND('',#580,.T.);
#332=FACE_BOUND('',#582,.T.);
#333=FACE_BOUND('',#583,.T.);
#334=FACE_BOUND('',#594,.T.);
#335=FACE_BOUND('',#595,.T.);
#336=FACE_BOUND('',#597,.T.);
#337=FACE_BOUND('',#598,.T.);
#338=FACE_BOUND('',#606,.T.);
#339=FACE_BOUND('',#607,.T.);
#340=FACE_BOUND('',#609,.T.);
#341=FACE_BOUND('',#610,.T.);
#342=FACE_BOUND('',#613,.T.);
#343=FACE_BOUND('',#615,.T.);
#344=FACE_BOUND('',#618,.T.);
#345=FACE_BOUND('',#625,.T.);
#346=FACE_BOUND('',#627,.T.);
#347=FACE_BOUND('',#630,.T.);
#348=FACE_BOUND('',#638,.T.);
#349=FACE_BOUND('',#640,.T.);
#350=FACE_BOUND('',#643,.T.);
#351=FACE_BOUND('',#645,.T.);
#352=FACE_BOUND('',#648,.T.);
#353=FACE_BOUND('',#651,.T.);
#354=FACE_BOUND('',#655,.T.);
#355=FACE_BOUND('',#659,.T.);
#356=FACE_BOUND('',#661,.T.);
#357=FACE_BOUND('',#667,.T.);
#358=FACE_BOUND('',#669,.T.);
#359=FACE_BOUND('',#672,.T.);
#360=FACE_BOUND('',#680,.T.);
#361=FACE_BOUND('',#682,.T.);
#362=FACE_BOUND('',#686,.T.);
#363=FACE_BOUND('',#688,.T.);
#364=PLANE('',#2090);
#365=PLANE('',#2091);
#366=PLANE('',#2092);
#367=PLANE('',#2093);
#368=PLANE('',#2094);
#369=PLANE('',#2095);
#370=PLANE('',#2103);
#371=PLANE('',#2104);
#372=PLANE('',#2109);
#373=PLANE('',#2110);
#374=PLANE('',#2111);
#375=PLANE('',#2112);
#376=PLANE('',#2113);
#377=PLANE('',#2114);
#378=PLANE('',#2122);
#379=PLANE('',#2126);
#380=PLANE('',#2130);
#381=PLANE('',#2131);
#382=PLANE('',#2136);
#383=PLANE('',#2137);
#384=PLANE('',#2145);
#385=PLANE('',#2149);
#386=PLANE('',#2153);
#387=PLANE('',#2154);
#388=PLANE('',#2162);
#389=PLANE('',#2166);
#390=PLANE('',#2170);
#391=PLANE('',#2171);
#392=PLANE('',#2176);
#393=PLANE('',#2178);
#394=PLANE('',#2182);
#395=PLANE('',#2187);
#396=PLANE('',#2189);
#397=PLANE('',#2194);
#398=PLANE('',#2196);
#399=PLANE('',#2200);
#400=PLANE('',#2205);
#401=PLANE('',#2207);
#402=PLANE('',#2215);
#403=PLANE('',#2216);
#404=PLANE('',#2221);
#405=PLANE('',#2223);
#406=PLANE('',#2227);
#407=PLANE('',#2232);
#408=PLANE('',#2237);
#409=PLANE('',#2245);
#410=PLANE('',#2246);
#411=PLANE('',#2251);
#412=PLANE('',#2257);
#413=PLANE('',#2259);
#414=PLANE('',#2263);
#415=PLANE('',#2268);
#416=PLANE('',#2270);
#417=PLANE('',#2278);
#418=PLANE('',#2279);
#419=PLANE('',#2287);
#420=PLANE('',#2288);
#421=PLANE('',#2290);
#422=PLANE('',#2291);
#423=PLANE('',#2292);
#424=PLANE('',#2299);
#425=FACE_OUTER_BOUND('',#536,.T.);
#426=FACE_OUTER_BOUND('',#537,.T.);
#427=FACE_OUTER_BOUND('',#538,.T.);
#428=FACE_OUTER_BOUND('',#539,.T.);
#429=FACE_OUTER_BOUND('',#540,.T.);
#430=FACE_OUTER_BOUND('',#541,.T.);
#431=FACE_OUTER_BOUND('',#542,.T.);
#432=FACE_OUTER_BOUND('',#543,.T.);
#433=FACE_OUTER_BOUND('',#544,.T.);
#434=FACE_OUTER_BOUND('',#545,.T.);
#435=FACE_OUTER_BOUND('',#551,.T.);
#436=FACE_OUTER_BOUND('',#557,.T.);
#437=FACE_OUTER_BOUND('',#558,.T.);
#438=FACE_OUTER_BOUND('',#559,.T.);
#439=FACE_OUTER_BOUND('',#561,.T.);
#440=FACE_OUTER_BOUND('',#563,.T.);
#441=FACE_OUTER_BOUND('',#564,.T.);
#442=FACE_OUTER_BOUND('',#565,.T.);
#443=FACE_OUTER_BOUND('',#566,.T.);
#444=FACE_OUTER_BOUND('',#567,.T.);
#445=FACE_OUTER_BOUND('',#568,.T.);
#446=FACE_OUTER_BOUND('',#570,.T.);
#447=FACE_OUTER_BOUND('',#572,.T.);
#448=FACE_OUTER_BOUND('',#573,.T.);
#449=FACE_OUTER_BOUND('',#574,.T.);
#450=FACE_OUTER_BOUND('',#575,.T.);
#451=FACE_OUTER_BOUND('',#576,.T.);
#452=FACE_OUTER_BOUND('',#577,.T.);
#453=FACE_OUTER_BOUND('',#578,.T.);
#454=FACE_OUTER_BOUND('',#581,.T.);
#455=FACE_OUTER_BOUND('',#584,.T.);
#456=FACE_OUTER_BOUND('',#585,.T.);
#457=FACE_OUTER_BOUND('',#586,.T.);
#458=FACE_OUTER_BOUND('',#587,.T.);
#459=FACE_OUTER_BOUND('',#588,.T.);
#460=FACE_OUTER_BOUND('',#589,.T.);
#461=FACE_OUTER_BOUND('',#590,.T.);
#462=FACE_OUTER_BOUND('',#591,.T.);
#463=FACE_OUTER_BOUND('',#592,.T.);
#464=FACE_OUTER_BOUND('',#593,.T.);
#465=FACE_OUTER_BOUND('',#596,.T.);
#466=FACE_OUTER_BOUND('',#599,.T.);
#467=FACE_OUTER_BOUND('',#600,.T.);
#468=FACE_OUTER_BOUND('',#601,.T.);
#469=FACE_OUTER_BOUND('',#602,.T.);
#470=FACE_OUTER_BOUND('',#603,.T.);
#471=FACE_OUTER_BOUND('',#604,.T.);
#472=FACE_OUTER_BOUND('',#605,.T.);
#473=FACE_OUTER_BOUND('',#608,.T.);
#474=FACE_OUTER_BOUND('',#611,.T.);
#475=FACE_OUTER_BOUND('',#612,.T.);
#476=FACE_OUTER_BOUND('',#614,.T.);
#477=FACE_OUTER_BOUND('',#616,.T.);
#478=FACE_OUTER_BOUND('',#617,.T.);
#479=FACE_OUTER_BOUND('',#619,.T.);
#480=FACE_OUTER_BOUND('',#620,.T.);
#481=FACE_OUTER_BOUND('',#621,.T.);
#482=FACE_OUTER_BOUND('',#622,.T.);
#483=FACE_OUTER_BOUND('',#623,.T.);
#484=FACE_OUTER_BOUND('',#624,.T.);
#485=FACE_OUTER_BOUND('',#626,.T.);
#486=FACE_OUTER_BOUND('',#628,.T.);
#487=FACE_OUTER_BOUND('',#629,.T.);
#488=FACE_OUTER_BOUND('',#631,.T.);
#489=FACE_OUTER_BOUND('',#632,.T.);
#490=FACE_OUTER_BOUND('',#633,.T.);
#491=FACE_OUTER_BOUND('',#634,.T.);
#492=FACE_OUTER_BOUND('',#635,.T.);
#493=FACE_OUTER_BOUND('',#636,.T.);
#494=FACE_OUTER_BOUND('',#637,.T.);
#495=FACE_OUTER_BOUND('',#639,.T.);
#496=FACE_OUTER_BOUND('',#641,.T.);
#497=FACE_OUTER_BOUND('',#642,.T.);
#498=FACE_OUTER_BOUND('',#644,.T.);
#499=FACE_OUTER_BOUND('',#646,.T.);
#500=FACE_OUTER_BOUND('',#647,.T.);
#501=FACE_OUTER_BOUND('',#649,.T.);
#502=FACE_OUTER_BOUND('',#650,.T.);
#503=FACE_OUTER_BOUND('',#652,.T.);
#504=FACE_OUTER_BOUND('',#653,.T.);
#505=FACE_OUTER_BOUND('',#654,.T.);
#506=FACE_OUTER_BOUND('',#656,.T.);
#507=FACE_OUTER_BOUND('',#657,.T.);
#508=FACE_OUTER_BOUND('',#658,.T.);
#509=FACE_OUTER_BOUND('',#660,.T.);
#510=FACE_OUTER_BOUND('',#662,.T.);
#511=FACE_OUTER_BOUND('',#663,.T.);
#512=FACE_OUTER_BOUND('',#664,.T.);
#513=FACE_OUTER_BOUND('',#665,.T.);
#514=FACE_OUTER_BOUND('',#666,.T.);
#515=FACE_OUTER_BOUND('',#668,.T.);
#516=FACE_OUTER_BOUND('',#670,.T.);
#517=FACE_OUTER_BOUND('',#671,.T.);
#518=FACE_OUTER_BOUND('',#673,.T.);
#519=FACE_OUTER_BOUND('',#674,.T.);
#520=FACE_OUTER_BOUND('',#675,.T.);
#521=FACE_OUTER_BOUND('',#676,.T.);
#522=FACE_OUTER_BOUND('',#677,.T.);
#523=FACE_OUTER_BOUND('',#678,.T.);
#524=FACE_OUTER_BOUND('',#679,.T.);
#525=FACE_OUTER_BOUND('',#681,.T.);
#526=FACE_OUTER_BOUND('',#683,.T.);
#527=FACE_OUTER_BOUND('',#684,.T.);
#528=FACE_OUTER_BOUND('',#685,.T.);
#529=FACE_OUTER_BOUND('',#687,.T.);
#530=FACE_OUTER_BOUND('',#689,.T.);
#531=FACE_OUTER_BOUND('',#690,.T.);
#532=FACE_OUTER_BOUND('',#691,.T.);
#533=FACE_OUTER_BOUND('',#692,.T.);
#534=FACE_OUTER_BOUND('',#693,.T.);
#535=FACE_OUTER_BOUND('',#694,.T.);
#536=EDGE_LOOP('',(#1316,#1317,#1318,#1319));
#537=EDGE_LOOP('',(#1320,#1321,#1322,#1323));
#538=EDGE_LOOP('',(#1324,#1325,#1326,#1327));
#539=EDGE_LOOP('',(#1328,#1329,#1330,#1331));
#540=EDGE_LOOP('',(#1332,#1333,#1334,#1335));
#541=EDGE_LOOP('',(#1336,#1337,#1338,#1339));
#542=EDGE_LOOP('',(#1340,#1341,#1342,#1343));
#543=EDGE_LOOP('',(#1344,#1345,#1346,#1347));
#544=EDGE_LOOP('',(#1348,#1349,#1350,#1351));
#545=EDGE_LOOP('',(#1352,#1353,#1354,#1355));
#546=EDGE_LOOP('',(#1356));
#547=EDGE_LOOP('',(#1357));
#548=EDGE_LOOP('',(#1358));
#549=EDGE_LOOP('',(#1359));
#550=EDGE_LOOP('',(#1360));
#551=EDGE_LOOP('',(#1361,#1362,#1363,#1364));
#552=EDGE_LOOP('',(#1365));
#553=EDGE_LOOP('',(#1366));
#554=EDGE_LOOP('',(#1367));
#555=EDGE_LOOP('',(#1368));
#556=EDGE_LOOP('',(#1369));
#557=EDGE_LOOP('',(#1370,#1371,#1372,#1373));
#558=EDGE_LOOP('',(#1374,#1375,#1376,#1377));
#559=EDGE_LOOP('',(#1378));
#560=EDGE_LOOP('',(#1379));
#561=EDGE_LOOP('',(#1380));
#562=EDGE_LOOP('',(#1381));
#563=EDGE_LOOP('',(#1382,#1383,#1384,#1385));
#564=EDGE_LOOP('',(#1386,#1387,#1388,#1389));
#565=EDGE_LOOP('',(#1390,#1391,#1392,#1393));
#566=EDGE_LOOP('',(#1394,#1395,#1396,#1397));
#567=EDGE_LOOP('',(#1398,#1399,#1400,#1401));
#568=EDGE_LOOP('',(#1402,#1403,#1404,#1405));
#569=EDGE_LOOP('',(#1406));
#570=EDGE_LOOP('',(#1407,#1408,#1409,#1410));
#571=EDGE_LOOP('',(#1411));
#572=EDGE_LOOP('',(#1412,#1413,#1414,#1415));
#573=EDGE_LOOP('',(#1416,#1417,#1418,#1419));
#574=EDGE_LOOP('',(#1420,#1421,#1422,#1423));
#575=EDGE_LOOP('',(#1424,#1425,#1426,#1427));
#576=EDGE_LOOP('',(#1428,#1429,#1430,#1431));
#577=EDGE_LOOP('',(#1432,#1433,#1434,#1435));
#578=EDGE_LOOP('',(#1436,#1437,#1438,#1439));
#579=EDGE_LOOP('',(#1440));
#580=EDGE_LOOP('',(#1441));
#581=EDGE_LOOP('',(#1442,#1443,#1444,#1445));
#582=EDGE_LOOP('',(#1446));
#583=EDGE_LOOP('',(#1447));
#584=EDGE_LOOP('',(#1448,#1449,#1450,#1451));
#585=EDGE_LOOP('',(#1452));
#586=EDGE_LOOP('',(#1453));
#587=EDGE_LOOP('',(#1454,#1455,#1456,#1457));
#588=EDGE_LOOP('',(#1458,#1459,#1460,#1461));
#589=EDGE_LOOP('',(#1462,#1463,#1464,#1465));
#590=EDGE_LOOP('',(#1466,#1467,#1468,#1469));
#591=EDGE_LOOP('',(#1470,#1471,#1472,#1473));
#592=EDGE_LOOP('',(#1474,#1475,#1476,#1477));
#593=EDGE_LOOP('',(#1478,#1479,#1480,#1481));
#594=EDGE_LOOP('',(#1482));
#595=EDGE_LOOP('',(#1483));
#596=EDGE_LOOP('',(#1484,#1485,#1486,#1487));
#597=EDGE_LOOP('',(#1488));
#598=EDGE_LOOP('',(#1489));
#599=EDGE_LOOP('',(#1490,#1491,#1492,#1493));
#600=EDGE_LOOP('',(#1494,#1495,#1496,#1497));
#601=EDGE_LOOP('',(#1498,#1499,#1500,#1501));
#602=EDGE_LOOP('',(#1502,#1503,#1504,#1505));
#603=EDGE_LOOP('',(#1506,#1507,#1508,#1509));
#604=EDGE_LOOP('',(#1510,#1511,#1512,#1513));
#605=EDGE_LOOP('',(#1514,#1515,#1516,#1517));
#606=EDGE_LOOP('',(#1518));
#607=EDGE_LOOP('',(#1519));
#608=EDGE_LOOP('',(#1520,#1521,#1522,#1523));
#609=EDGE_LOOP('',(#1524));
#610=EDGE_LOOP('',(#1525));
#611=EDGE_LOOP('',(#1526,#1527,#1528,#1529));
#612=EDGE_LOOP('',(#1530));
#613=EDGE_LOOP('',(#1531));
#614=EDGE_LOOP('',(#1532));
#615=EDGE_LOOP('',(#1533));
#616=EDGE_LOOP('',(#1534,#1535,#1536,#1537));
#617=EDGE_LOOP('',(#1538));
#618=EDGE_LOOP('',(#1539));
#619=EDGE_LOOP('',(#1540,#1541,#1542,#1543));
#620=EDGE_LOOP('',(#1544));
#621=EDGE_LOOP('',(#1545,#1546,#1547,#1548));
#622=EDGE_LOOP('',(#1549));
#623=EDGE_LOOP('',(#1550,#1551,#1552,#1553));
#624=EDGE_LOOP('',(#1554));
#625=EDGE_LOOP('',(#1555));
#626=EDGE_LOOP('',(#1556));
#627=EDGE_LOOP('',(#1557));
#628=EDGE_LOOP('',(#1558,#1559,#1560,#1561));
#629=EDGE_LOOP('',(#1562));
#630=EDGE_LOOP('',(#1563));
#631=EDGE_LOOP('',(#1564,#1565,#1566,#1567));
#632=EDGE_LOOP('',(#1568));
#633=EDGE_LOOP('',(#1569,#1570,#1571,#1572));
#634=EDGE_LOOP('',(#1573));
#635=EDGE_LOOP('',(#1574,#1575,#1576,#1577));
#636=EDGE_LOOP('',(#1578,#1579,#1580,#1581));
#637=EDGE_LOOP('',(#1582));
#638=EDGE_LOOP('',(#1583));
#639=EDGE_LOOP('',(#1584));
#640=EDGE_LOOP('',(#1585));
#641=EDGE_LOOP('',(#1586,#1587,#1588,#1589));
#642=EDGE_LOOP('',(#1590));
#643=EDGE_LOOP('',(#1591));
#644=EDGE_LOOP('',(#1592));
#645=EDGE_LOOP('',(#1593));
#646=EDGE_LOOP('',(#1594,#1595,#1596,#1597));
#647=EDGE_LOOP('',(#1598));
#648=EDGE_LOOP('',(#1599));
#649=EDGE_LOOP('',(#1600,#1601,#1602,#1603));
#650=EDGE_LOOP('',(#1604));
#651=EDGE_LOOP('',(#1605));
#652=EDGE_LOOP('',(#1606,#1607,#1608,#1609));
#653=EDGE_LOOP('',(#1610,#1611,#1612,#1613));
#654=EDGE_LOOP('',(#1614));
#655=EDGE_LOOP('',(#1615));
#656=EDGE_LOOP('',(#1616,#1617,#1618,#1619));
#657=EDGE_LOOP('',(#1620,#1621,#1622,#1623));
#658=EDGE_LOOP('',(#1624));
#659=EDGE_LOOP('',(#1625));
#660=EDGE_LOOP('',(#1626));
#661=EDGE_LOOP('',(#1627));
#662=EDGE_LOOP('',(#1628,#1629,#1630,#1631));
#663=EDGE_LOOP('',(#1632));
#664=EDGE_LOOP('',(#1633,#1634,#1635));
#665=EDGE_LOOP('',(#1636,#1637,#1638,#1639));
#666=EDGE_LOOP('',(#1640));
#667=EDGE_LOOP('',(#1641));
#668=EDGE_LOOP('',(#1642));
#669=EDGE_LOOP('',(#1643));
#670=EDGE_LOOP('',(#1644,#1645,#1646,#1647));
#671=EDGE_LOOP('',(#1648));
#672=EDGE_LOOP('',(#1649));
#673=EDGE_LOOP('',(#1650,#1651,#1652,#1653));
#674=EDGE_LOOP('',(#1654));
#675=EDGE_LOOP('',(#1655,#1656,#1657,#1658));
#676=EDGE_LOOP('',(#1659));
#677=EDGE_LOOP('',(#1660,#1661,#1662,#1663));
#678=EDGE_LOOP('',(#1664,#1665,#1666,#1667));
#679=EDGE_LOOP('',(#1668));
#680=EDGE_LOOP('',(#1669));
#681=EDGE_LOOP('',(#1670));
#682=EDGE_LOOP('',(#1671));
#683=EDGE_LOOP('',(#1672,#1673,#1674,#1675));
#684=EDGE_LOOP('',(#1676,#1677,#1678,#1679));
#685=EDGE_LOOP('',(#1680));
#686=EDGE_LOOP('',(#1681));
#687=EDGE_LOOP('',(#1682));
#688=EDGE_LOOP('',(#1683));
#689=EDGE_LOOP('',(#1684,#1685,#1686,#1687));
#690=EDGE_LOOP('',(#1688,#1689,#1690,#1691));
#691=EDGE_LOOP('',(#1692,#1693,#1694,#1695));
#692=EDGE_LOOP('',(#1696,#1697,#1698,#1699));
#693=EDGE_LOOP('',(#1700,#1701,#1702,#1703));
#694=EDGE_LOOP('',(#1704,#1705,#1706,#1707));
#695=LINE('',#3035,#793);
#696=LINE('',#3041,#794);
#697=LINE('',#3047,#795);
#698=LINE('',#3053,#796);
#699=LINE('',#3059,#797);
#700=LINE('',#3064,#798);
#701=LINE('',#3066,#799);
#702=LINE('',#3068,#800);
#703=LINE('',#3069,#801);
#704=LINE('',#3072,#802);
#705=LINE('',#3074,#803);
#706=LINE('',#3075,#804);
#707=LINE('',#3078,#805);
#708=LINE('',#3080,#806);
#709=LINE('',#3081,#807);
#710=LINE('',#3083,#808);
#711=LINE('',#3084,#809);
#712=LINE('',#3092,#810);
#713=LINE('',#3098,#811);
#714=LINE('',#3107,#812);
#715=LINE('',#3112,#813);
#716=LINE('',#3114,#814);
#717=LINE('',#3116,#815);
#718=LINE('',#3117,#816);
#719=LINE('',#3120,#817);
#720=LINE('',#3122,#818);
#721=LINE('',#3123,#819);
#722=LINE('',#3126,#820);
#723=LINE('',#3128,#821);
#724=LINE('',#3129,#822);
#725=LINE('',#3131,#823);
#726=LINE('',#3132,#824);
#727=LINE('',#3140,#825);
#728=LINE('',#3146,#826);
#729=LINE('',#3151,#827);
#730=LINE('',#3153,#828);
#731=LINE('',#3155,#829);
#732=LINE('',#3156,#830);
#733=LINE('',#3162,#831);
#734=LINE('',#3165,#832);
#735=LINE('',#3167,#833);
#736=LINE('',#3168,#834);
#737=LINE('',#3179,#835);
#738=LINE('',#3188,#836);
#739=LINE('',#3194,#837);
#740=LINE('',#3199,#838);
#741=LINE('',#3201,#839);
#742=LINE('',#3203,#840);
#743=LINE('',#3204,#841);
#744=LINE('',#3210,#842);
#745=LINE('',#3213,#843);
#746=LINE('',#3215,#844);
#747=LINE('',#3216,#845);
#748=LINE('',#3227,#846);
#749=LINE('',#3233,#847);
#750=LINE('',#3238,#848);
#751=LINE('',#3240,#849);
#752=LINE('',#3242,#850);
#753=LINE('',#3243,#851);
#754=LINE('',#3249,#852);
#755=LINE('',#3252,#853);
#756=LINE('',#3254,#854);
#757=LINE('',#3255,#855);
#758=LINE('',#3266,#856);
#759=LINE('',#3277,#857);
#760=LINE('',#3285,#858);
#761=LINE('',#3289,#859);
#762=LINE('',#3296,#860);
#763=LINE('',#3307,#861);
#764=LINE('',#3315,#862);
#765=LINE('',#3319,#863);
#766=LINE('',#3326,#864);
#767=LINE('',#3332,#865);
#768=LINE('',#3341,#866);
#769=LINE('',#3352,#867);
#770=LINE('',#3360,#868);
#771=LINE('',#3368,#869);
#772=LINE('',#3370,#870);
#773=LINE('',#3377,#871);
#774=LINE('',#3383,#872);
#775=LINE('',#3392,#873);
#776=LINE('',#3397,#874);
#777=LINE('',#3403,#875);
#778=LINE('',#3414,#876);
#779=LINE('',#3422,#877);
#780=LINE('',#3426,#878);
#781=LINE('',#3433,#879);
#782=LINE('',#3439,#880);
#783=LINE('',#3448,#881);
#784=LINE('',#3454,#882);
#785=LINE('',#3462,#883);
#786=LINE('',#3464,#884);
#787=LINE('',#3466,#885);
#788=LINE('',#3467,#886);
#789=LINE('',#3471,#887);
#790=LINE('',#3473,#888);
#791=LINE('',#3475,#889);
#792=LINE('',#3476,#890);
#793=VECTOR('',#2367,4.5);
#794=VECTOR('',#2374,4.5);
#795=VECTOR('',#2381,4.5);
#796=VECTOR('',#2388,4.5);
#797=VECTOR('',#2395,5.);
#798=VECTOR('',#2400,10.);
#799=VECTOR('',#2401,10.);
#800=VECTOR('',#2402,10.);
#801=VECTOR('',#2403,10.);
#802=VECTOR('',#2406,10.);
#803=VECTOR('',#2407,10.);
#804=VECTOR('',#2408,10.);
#805=VECTOR('',#2411,10.);
#806=VECTOR('',#2412,10.);
#807=VECTOR('',#2413,10.);
#808=VECTOR('',#2416,10.);
#809=VECTOR('',#2417,10.);
#810=VECTOR('',#2428,5.);
#811=VECTOR('',#2435,12.);
#812=VECTOR('',#2448,5.);
#813=VECTOR('',#2453,10.);
#814=VECTOR('',#2454,10.);
#815=VECTOR('',#2455,10.);
#816=VECTOR('',#2456,10.);
#817=VECTOR('',#2459,10.);
#818=VECTOR('',#2460,10.);
#819=VECTOR('',#2461,10.);
#820=VECTOR('',#2464,10.);
#821=VECTOR('',#2465,10.);
#822=VECTOR('',#2466,10.);
#823=VECTOR('',#2469,10.);
#824=VECTOR('',#2470,10.);
#825=VECTOR('',#2481,7.);
#826=VECTOR('',#2488,7.);
#827=VECTOR('',#2493,10.);
#828=VECTOR('',#2494,10.);
#829=VECTOR('',#2495,10.);
#830=VECTOR('',#2496,10.);
#831=VECTOR('',#2503,10.);
#832=VECTOR('',#2506,10.);
#833=VECTOR('',#2507,10.);
#834=VECTOR('',#2508,10.);
#835=VECTOR('',#2525,8.);
#836=VECTOR('',#2538,7.);
#837=VECTOR('',#2545,7.);
#838=VECTOR('',#2550,10.);
#839=VECTOR('',#2551,10.);
#840=VECTOR('',#2552,10.);
#841=VECTOR('',#2553,10.);
#842=VECTOR('',#2560,10.);
#843=VECTOR('',#2563,10.);
#844=VECTOR('',#2564,10.);
#845=VECTOR('',#2565,10.);
#846=VECTOR('',#2582,7.);
#847=VECTOR('',#2589,7.);
#848=VECTOR('',#2594,10.);
#849=VECTOR('',#2595,10.);
#850=VECTOR('',#2596,10.);
#851=VECTOR('',#2597,10.);
#852=VECTOR('',#2604,10.);
#853=VECTOR('',#2607,10.);
#854=VECTOR('',#2608,10.);
#855=VECTOR('',#2609,10.);
#856=VECTOR('',#2626,4.);
#857=VECTOR('',#2641,5.);
#858=VECTOR('',#2650,8.);
#859=VECTOR('',#2657,5.);
#860=VECTOR('',#2666,4.);
#861=VECTOR('',#2681,5.);
#862=VECTOR('',#2690,8.);
#863=VECTOR('',#2697,5.);
#864=VECTOR('',#2706,5.);
#865=VECTOR('',#2713,7.);
#866=VECTOR('',#2726,4.);
#867=VECTOR('',#2741,5.);
#868=VECTOR('',#2750,8.);
#869=VECTOR('',#2761,2.);
#870=VECTOR('',#2764,5.);
#871=VECTOR('',#2773,5.);
#872=VECTOR('',#2780,7.);
#873=VECTOR('',#2793,2.);
#874=VECTOR('',#2800,1.);
#875=VECTOR('',#2807,4.);
#876=VECTOR('',#2822,5.);
#877=VECTOR('',#2831,8.);
#878=VECTOR('',#2838,5.);
#879=VECTOR('',#2847,5.);
#880=VECTOR('',#2854,7.);
#881=VECTOR('',#2867,5.);
#882=VECTOR('',#2874,10.);
#883=VECTOR('',#2885,10.);
#884=VECTOR('',#2886,10.);
#885=VECTOR('',#2887,10.);
#886=VECTOR('',#2888,10.);
#887=VECTOR('',#2891,10.);
#888=VECTOR('',#2892,10.);
#889=VECTOR('',#2893,10.);
#890=VECTOR('',#2894,10.);
#891=CIRCLE('',#2076,4.5);
#892=CIRCLE('',#2077,4.5);
#893=CIRCLE('',#2079,4.5);
#894=CIRCLE('',#2080,4.5);
#895=CIRCLE('',#2082,4.5);
#896=CIRCLE('',#2083,4.5);
#897=CIRCLE('',#2085,4.5);
#898=CIRCLE('',#2086,4.5);
#899=CIRCLE('',#2088,5.);
#900=CIRCLE('',#2089,5.);
#901=CIRCLE('',#2098,5.);
#902=CIRCLE('',#2099,5.);
#903=CIRCLE('',#2101,17.);
#904=CIRCLE('',#2102,17.);
#905=CIRCLE('',#2107,5.);
#906=CIRCLE('',#2108,5.);
#907=CIRCLE('',#2117,7.);
#908=CIRCLE('',#2118,7.);
#909=CIRCLE('',#2120,7.);
#910=CIRCLE('',#2121,7.);
#911=CIRCLE('',#2124,12.);
#912=CIRCLE('',#2125,12.);
#913=CIRCLE('',#2128,12.);
#914=CIRCLE('',#2129,12.);
#915=CIRCLE('',#2134,8.);
#916=CIRCLE('',#2135,8.);
#917=CIRCLE('',#2140,7.);
#918=CIRCLE('',#2141,7.);
#919=CIRCLE('',#2143,7.);
#920=CIRCLE('',#2144,7.);
#921=CIRCLE('',#2147,12.);
#922=CIRCLE('',#2148,12.);
#923=CIRCLE('',#2151,12.);
#924=CIRCLE('',#2152,12.);
#925=CIRCLE('',#2157,7.);
#926=CIRCLE('',#2158,7.);
#927=CIRCLE('',#2160,7.);
#928=CIRCLE('',#2161,7.);
#929=CIRCLE('',#2164,12.);
#930=CIRCLE('',#2165,12.);
#931=CIRCLE('',#2168,12.);
#932=CIRCLE('',#2169,12.);
#933=CIRCLE('',#2174,4.);
#934=CIRCLE('',#2175,4.);
#935=CIRCLE('',#2177,5.);
#936=CIRCLE('',#2179,5.);
#937=CIRCLE('',#2181,5.);
#938=CIRCLE('',#2183,8.);
#939=CIRCLE('',#2184,5.);
#940=CIRCLE('',#2186,8.);
#941=CIRCLE('',#2192,4.);
#942=CIRCLE('',#2193,4.);
#943=CIRCLE('',#2195,5.);
#944=CIRCLE('',#2197,5.);
#945=CIRCLE('',#2199,5.);
#946=CIRCLE('',#2201,8.);
#947=CIRCLE('',#2202,5.);
#948=CIRCLE('',#2204,8.);
#949=CIRCLE('',#2210,5.);
#950=CIRCLE('',#2211,5.);
#951=CIRCLE('',#2213,7.);
#952=CIRCLE('',#2214,7.);
#953=CIRCLE('',#2219,4.);
#954=CIRCLE('',#2220,4.);
#955=CIRCLE('',#2222,5.);
#956=CIRCLE('',#2224,5.);
#957=CIRCLE('',#2226,5.);
#958=CIRCLE('',#2228,8.);
#959=CIRCLE('',#2229,5.);
#960=CIRCLE('',#2231,8.);
#961=CIRCLE('',#2233,2.);
#962=CIRCLE('',#2235,2.);
#963=CIRCLE('',#2240,5.);
#964=CIRCLE('',#2241,5.);
#965=CIRCLE('',#2243,7.);
#966=CIRCLE('',#2244,7.);
#967=CIRCLE('',#2249,2.);
#968=CIRCLE('',#2250,2.);
#969=CIRCLE('',#2255,4.);
#970=CIRCLE('',#2256,4.);
#971=CIRCLE('',#2258,5.);
#972=CIRCLE('',#2260,5.);
#973=CIRCLE('',#2262,5.);
#974=CIRCLE('',#2264,8.);
#975=CIRCLE('',#2265,5.);
#976=CIRCLE('',#2267,8.);
#977=CIRCLE('',#2273,5.);
#978=CIRCLE('',#2274,5.);
#979=CIRCLE('',#2276,7.);
#980=CIRCLE('',#2277,7.);
#981=CIRCLE('',#2282,5.);
#982=CIRCLE('',#2283,5.);
#983=CIRCLE('',#2285,10.);
#984=CIRCLE('',#2286,10.);
#985=CIRCLE('',#2293,8.);
#986=CIRCLE('',#2294,4.);
#987=CIRCLE('',#2296,4.);
#988=CIRCLE('',#2298,8.);
#989=VERTEX_POINT('',#3032);
#990=VERTEX_POINT('',#3034);
#991=VERTEX_POINT('',#3038);
#992=VERTEX_POINT('',#3040);
#993=VERTEX_POINT('',#3044);
#994=VERTEX_POINT('',#3046);
#995=VERTEX_POINT('',#3050);
#996=VERTEX_POINT('',#3052);
#997=VERTEX_POINT('',#3056);
#998=VERTEX_POINT('',#3058);
#999=VERTEX_POINT('',#3062);
#1000=VERTEX_POINT('',#3063);
#1001=VERTEX_POINT('',#3065);
#1002=VERTEX_POINT('',#3067);
#1003=VERTEX_POINT('',#3071);
#1004=VERTEX_POINT('',#3073);
#1005=VERTEX_POINT('',#3077);
#1006=VERTEX_POINT('',#3079);
#1007=VERTEX_POINT('',#3089);
#1008=VERTEX_POINT('',#3091);
#1009=VERTEX_POINT('',#3095);
#1010=VERTEX_POINT('',#3097);
#1011=VERTEX_POINT('',#3104);
#1012=VERTEX_POINT('',#3106);
#1013=VERTEX_POINT('',#3110);
#1014=VERTEX_POINT('',#3111);
#1015=VERTEX_POINT('',#3113);
#1016=VERTEX_POINT('',#3115);
#1017=VERTEX_POINT('',#3119);
#1018=VERTEX_POINT('',#3121);
#1019=VERTEX_POINT('',#3125);
#1020=VERTEX_POINT('',#3127);
#1021=VERTEX_POINT('',#3137);
#1022=VERTEX_POINT('',#3139);
#1023=VERTEX_POINT('',#3143);
#1024=VERTEX_POINT('',#3145);
#1025=VERTEX_POINT('',#3149);
#1026=VERTEX_POINT('',#3150);
#1027=VERTEX_POINT('',#3152);
#1028=VERTEX_POINT('',#3154);
#1029=VERTEX_POINT('',#3158);
#1030=VERTEX_POINT('',#3160);
#1031=VERTEX_POINT('',#3164);
#1032=VERTEX_POINT('',#3166);
#1033=VERTEX_POINT('',#3176);
#1034=VERTEX_POINT('',#3178);
#1035=VERTEX_POINT('',#3185);
#1036=VERTEX_POINT('',#3187);
#1037=VERTEX_POINT('',#3191);
#1038=VERTEX_POINT('',#3193);
#1039=VERTEX_POINT('',#3197);
#1040=VERTEX_POINT('',#3198);
#1041=VERTEX_POINT('',#3200);
#1042=VERTEX_POINT('',#3202);
#1043=VERTEX_POINT('',#3206);
#1044=VERTEX_POINT('',#3208);
#1045=VERTEX_POINT('',#3212);
#1046=VERTEX_POINT('',#3214);
#1047=VERTEX_POINT('',#3224);
#1048=VERTEX_POINT('',#3226);
#1049=VERTEX_POINT('',#3230);
#1050=VERTEX_POINT('',#3232);
#1051=VERTEX_POINT('',#3236);
#1052=VERTEX_POINT('',#3237);
#1053=VERTEX_POINT('',#3239);
#1054=VERTEX_POINT('',#3241);
#1055=VERTEX_POINT('',#3245);
#1056=VERTEX_POINT('',#3247);
#1057=VERTEX_POINT('',#3251);
#1058=VERTEX_POINT('',#3253);
#1059=VERTEX_POINT('',#3263);
#1060=VERTEX_POINT('',#3265);
#1061=VERTEX_POINT('',#3269);
#1062=VERTEX_POINT('',#3272);
#1063=VERTEX_POINT('',#3275);
#1064=VERTEX_POINT('',#3279);
#1065=VERTEX_POINT('',#3281);
#1066=VERTEX_POINT('',#3284);
#1067=VERTEX_POINT('',#3293);
#1068=VERTEX_POINT('',#3295);
#1069=VERTEX_POINT('',#3299);
#1070=VERTEX_POINT('',#3302);
#1071=VERTEX_POINT('',#3305);
#1072=VERTEX_POINT('',#3309);
#1073=VERTEX_POINT('',#3311);
#1074=VERTEX_POINT('',#3314);
#1075=VERTEX_POINT('',#3323);
#1076=VERTEX_POINT('',#3325);
#1077=VERTEX_POINT('',#3329);
#1078=VERTEX_POINT('',#3331);
#1079=VERTEX_POINT('',#3338);
#1080=VERTEX_POINT('',#3340);
#1081=VERTEX_POINT('',#3344);
#1082=VERTEX_POINT('',#3347);
#1083=VERTEX_POINT('',#3350);
#1084=VERTEX_POINT('',#3354);
#1085=VERTEX_POINT('',#3356);
#1086=VERTEX_POINT('',#3359);
#1087=VERTEX_POINT('',#3363);
#1088=VERTEX_POINT('',#3366);
#1089=VERTEX_POINT('',#3374);
#1090=VERTEX_POINT('',#3376);
#1091=VERTEX_POINT('',#3380);
#1092=VERTEX_POINT('',#3382);
#1093=VERTEX_POINT('',#3389);
#1094=VERTEX_POINT('',#3391);
#1095=VERTEX_POINT('',#3396);
#1096=VERTEX_POINT('',#3400);
#1097=VERTEX_POINT('',#3402);
#1098=VERTEX_POINT('',#3406);
#1099=VERTEX_POINT('',#3409);
#1100=VERTEX_POINT('',#3412);
#1101=VERTEX_POINT('',#3416);
#1102=VERTEX_POINT('',#3418);
#1103=VERTEX_POINT('',#3421);
#1104=VERTEX_POINT('',#3430);
#1105=VERTEX_POINT('',#3432);
#1106=VERTEX_POINT('',#3436);
#1107=VERTEX_POINT('',#3438);
#1108=VERTEX_POINT('',#3445);
#1109=VERTEX_POINT('',#3447);
#1110=VERTEX_POINT('',#3451);
#1111=VERTEX_POINT('',#3453);
#1112=VERTEX_POINT('',#3460);
#1113=VERTEX_POINT('',#3461);
#1114=VERTEX_POINT('',#3463);
#1115=VERTEX_POINT('',#3465);
#1116=VERTEX_POINT('',#3469);
#1117=VERTEX_POINT('',#3470);
#1118=VERTEX_POINT('',#3472);
#1119=VERTEX_POINT('',#3474);
#1120=EDGE_CURVE('',#989,#989,#891,.T.);
#1121=EDGE_CURVE('',#989,#990,#695,.T.);
#1122=EDGE_CURVE('',#990,#990,#892,.T.);
#1123=EDGE_CURVE('',#991,#991,#893,.T.);
#1124=EDGE_CURVE('',#991,#992,#696,.T.);
#1125=EDGE_CURVE('',#992,#992,#894,.T.);
#1126=EDGE_CURVE('',#993,#993,#895,.T.);
#1127=EDGE_CURVE('',#993,#994,#697,.T.);
#1128=EDGE_CURVE('',#994,#994,#896,.T.);
#1129=EDGE_CURVE('',#995,#995,#897,.T.);
#1130=EDGE_CURVE('',#995,#996,#698,.T.);
#1131=EDGE_CURVE('',#996,#996,#898,.T.);
#1132=EDGE_CURVE('',#997,#997,#899,.T.);
#1133=EDGE_CURVE('',#997,#998,#699,.T.);
#1134=EDGE_CURVE('',#998,#998,#900,.T.);
#1135=EDGE_CURVE('',#999,#1000,#700,.F.);
#1136=EDGE_CURVE('',#1000,#1001,#701,.T.);
#1137=EDGE_CURVE('',#1002,#1001,#702,.F.);
#1138=EDGE_CURVE('',#999,#1002,#703,.F.);
#1139=EDGE_CURVE('',#1003,#999,#704,.F.);
#1140=EDGE_CURVE('',#1004,#1002,#705,.F.);
#1141=EDGE_CURVE('',#1003,#1004,#706,.F.);
#1142=EDGE_CURVE('',#1005,#1003,#707,.F.);
#1143=EDGE_CURVE('',#1006,#1004,#708,.F.);
#1144=EDGE_CURVE('',#1005,#1006,#709,.T.);
#1145=EDGE_CURVE('',#1000,#1005,#710,.F.);
#1146=EDGE_CURVE('',#1001,#1006,#711,.F.);
#1147=EDGE_CURVE('',#1007,#1007,#901,.T.);
#1148=EDGE_CURVE('',#1007,#1008,#712,.T.);
#1149=EDGE_CURVE('',#1008,#1008,#902,.T.);
#1150=EDGE_CURVE('',#1009,#1009,#903,.F.);
#1151=EDGE_CURVE('',#1009,#1010,#713,.T.);
#1152=EDGE_CURVE('',#1010,#1010,#904,.F.);
#1153=EDGE_CURVE('',#1011,#1011,#905,.T.);
#1154=EDGE_CURVE('',#1011,#1012,#714,.T.);
#1155=EDGE_CURVE('',#1012,#1012,#906,.T.);
#1156=EDGE_CURVE('',#1013,#1014,#715,.T.);
#1157=EDGE_CURVE('',#1014,#1015,#716,.T.);
#1158=EDGE_CURVE('',#1016,#1015,#717,.T.);
#1159=EDGE_CURVE('',#1013,#1016,#718,.T.);
#1160=EDGE_CURVE('',#1017,#1013,#719,.T.);
#1161=EDGE_CURVE('',#1018,#1016,#720,.T.);
#1162=EDGE_CURVE('',#1017,#1018,#721,.T.);
#1163=EDGE_CURVE('',#1019,#1017,#722,.T.);
#1164=EDGE_CURVE('',#1020,#1018,#723,.T.);
#1165=EDGE_CURVE('',#1019,#1020,#724,.T.);
#1166=EDGE_CURVE('',#1014,#1019,#725,.T.);
#1167=EDGE_CURVE('',#1015,#1020,#726,.T.);
#1168=EDGE_CURVE('',#1021,#1021,#907,.T.);
#1169=EDGE_CURVE('',#1021,#1022,#727,.T.);
#1170=EDGE_CURVE('',#1022,#1022,#908,.T.);
#1171=EDGE_CURVE('',#1023,#1023,#909,.T.);
#1172=EDGE_CURVE('',#1023,#1024,#728,.T.);
#1173=EDGE_CURVE('',#1024,#1024,#910,.T.);
#1174=EDGE_CURVE('',#1025,#1026,#729,.T.);
#1175=EDGE_CURVE('',#1026,#1027,#730,.T.);
#1176=EDGE_CURVE('',#1028,#1027,#731,.T.);
#1177=EDGE_CURVE('',#1025,#1028,#732,.T.);
#1178=EDGE_CURVE('',#1029,#1025,#911,.T.);
#1179=EDGE_CURVE('',#1030,#1028,#912,.T.);
#1180=EDGE_CURVE('',#1029,#1030,#733,.T.);
#1181=EDGE_CURVE('',#1031,#1029,#734,.T.);
#1182=EDGE_CURVE('',#1032,#1030,#735,.T.);
#1183=EDGE_CURVE('',#1031,#1032,#736,.T.);
#1184=EDGE_CURVE('',#1026,#1031,#913,.T.);
#1185=EDGE_CURVE('',#1027,#1032,#914,.T.);
#1186=EDGE_CURVE('',#1033,#1033,#915,.T.);
#1187=EDGE_CURVE('',#1033,#1034,#737,.T.);
#1188=EDGE_CURVE('',#1034,#1034,#916,.T.);
#1189=EDGE_CURVE('',#1035,#1035,#917,.T.);
#1190=EDGE_CURVE('',#1035,#1036,#738,.T.);
#1191=EDGE_CURVE('',#1036,#1036,#918,.T.);
#1192=EDGE_CURVE('',#1037,#1037,#919,.T.);
#1193=EDGE_CURVE('',#1037,#1038,#739,.T.);
#1194=EDGE_CURVE('',#1038,#1038,#920,.T.);
#1195=EDGE_CURVE('',#1039,#1040,#740,.T.);
#1196=EDGE_CURVE('',#1040,#1041,#741,.T.);
#1197=EDGE_CURVE('',#1042,#1041,#742,.T.);
#1198=EDGE_CURVE('',#1039,#1042,#743,.T.);
#1199=EDGE_CURVE('',#1043,#1039,#921,.T.);
#1200=EDGE_CURVE('',#1044,#1042,#922,.T.);
#1201=EDGE_CURVE('',#1043,#1044,#744,.T.);
#1202=EDGE_CURVE('',#1045,#1043,#745,.T.);
#1203=EDGE_CURVE('',#1046,#1044,#746,.T.);
#1204=EDGE_CURVE('',#1045,#1046,#747,.T.);
#1205=EDGE_CURVE('',#1040,#1045,#923,.T.);
#1206=EDGE_CURVE('',#1041,#1046,#924,.T.);
#1207=EDGE_CURVE('',#1047,#1047,#925,.T.);
#1208=EDGE_CURVE('',#1047,#1048,#748,.T.);
#1209=EDGE_CURVE('',#1048,#1048,#926,.T.);
#1210=EDGE_CURVE('',#1049,#1049,#927,.T.);
#1211=EDGE_CURVE('',#1049,#1050,#749,.T.);
#1212=EDGE_CURVE('',#1050,#1050,#928,.T.);
#1213=EDGE_CURVE('',#1051,#1052,#750,.T.);
#1214=EDGE_CURVE('',#1052,#1053,#751,.T.);
#1215=EDGE_CURVE('',#1054,#1053,#752,.T.);
#1216=EDGE_CURVE('',#1051,#1054,#753,.T.);
#1217=EDGE_CURVE('',#1055,#1051,#929,.T.);
#1218=EDGE_CURVE('',#1056,#1054,#930,.T.);
#1219=EDGE_CURVE('',#1055,#1056,#754,.T.);
#1220=EDGE_CURVE('',#1057,#1055,#755,.T.);
#1221=EDGE_CURVE('',#1058,#1056,#756,.T.);
#1222=EDGE_CURVE('',#1057,#1058,#757,.T.);
#1223=EDGE_CURVE('',#1052,#1057,#931,.T.);
#1224=EDGE_CURVE('',#1053,#1058,#932,.T.);
#1225=EDGE_CURVE('',#1059,#1059,#933,.T.);
#1226=EDGE_CURVE('',#1059,#1060,#758,.T.);
#1227=EDGE_CURVE('',#1060,#1060,#934,.T.);
#1228=EDGE_CURVE('',#1061,#1061,#935,.T.);
#1229=EDGE_CURVE('',#1062,#1062,#936,.T.);
#1230=EDGE_CURVE('',#1063,#1063,#937,.T.);
#1231=EDGE_CURVE('',#1063,#1062,#759,.T.);
#1232=EDGE_CURVE('',#1064,#1064,#938,.T.);
#1233=EDGE_CURVE('',#1065,#1065,#939,.T.);
#1234=EDGE_CURVE('',#1064,#1066,#760,.T.);
#1235=EDGE_CURVE('',#1066,#1066,#940,.T.);
#1236=EDGE_CURVE('',#1061,#1065,#761,.T.);
#1237=EDGE_CURVE('',#1067,#1067,#941,.T.);
#1238=EDGE_CURVE('',#1067,#1068,#762,.T.);
#1239=EDGE_CURVE('',#1068,#1068,#942,.T.);
#1240=EDGE_CURVE('',#1069,#1069,#943,.T.);
#1241=EDGE_CURVE('',#1070,#1070,#944,.T.);
#1242=EDGE_CURVE('',#1071,#1071,#945,.T.);
#1243=EDGE_CURVE('',#1071,#1070,#763,.T.);
#1244=EDGE_CURVE('',#1072,#1072,#946,.T.);
#1245=EDGE_CURVE('',#1073,#1073,#947,.T.);
#1246=EDGE_CURVE('',#1072,#1074,#764,.T.);
#1247=EDGE_CURVE('',#1074,#1074,#948,.T.);
#1248=EDGE_CURVE('',#1069,#1073,#765,.T.);
#1249=EDGE_CURVE('',#1075,#1075,#949,.T.);
#1250=EDGE_CURVE('',#1075,#1076,#766,.T.);
#1251=EDGE_CURVE('',#1076,#1076,#950,.T.);
#1252=EDGE_CURVE('',#1077,#1077,#951,.T.);
#1253=EDGE_CURVE('',#1077,#1078,#767,.T.);
#1254=EDGE_CURVE('',#1078,#1078,#952,.T.);
#1255=EDGE_CURVE('',#1079,#1079,#953,.T.);
#1256=EDGE_CURVE('',#1079,#1080,#768,.T.);
#1257=EDGE_CURVE('',#1080,#1080,#954,.T.);
#1258=EDGE_CURVE('',#1081,#1081,#955,.T.);
#1259=EDGE_CURVE('',#1082,#1082,#956,.T.);
#1260=EDGE_CURVE('',#1083,#1083,#957,.T.);
#1261=EDGE_CURVE('',#1083,#1082,#769,.T.);
#1262=EDGE_CURVE('',#1084,#1084,#958,.T.);
#1263=EDGE_CURVE('',#1085,#1085,#959,.T.);
#1264=EDGE_CURVE('',#1084,#1086,#770,.T.);
#1265=EDGE_CURVE('',#1086,#1086,#960,.T.);
#1266=EDGE_CURVE('',#1087,#1087,#961,.T.);
#1267=EDGE_CURVE('',#1088,#1088,#962,.T.);
#1268=EDGE_CURVE('',#1088,#1087,#771,.T.);
#1269=EDGE_CURVE('',#1081,#1085,#772,.T.);
#1270=EDGE_CURVE('',#1089,#1089,#963,.T.);
#1271=EDGE_CURVE('',#1089,#1090,#773,.T.);
#1272=EDGE_CURVE('',#1090,#1090,#964,.T.);
#1273=EDGE_CURVE('',#1091,#1091,#965,.T.);
#1274=EDGE_CURVE('',#1091,#1092,#774,.T.);
#1275=EDGE_CURVE('',#1092,#1092,#966,.T.);
#1276=EDGE_CURVE('',#1093,#1093,#967,.T.);
#1277=EDGE_CURVE('',#1093,#1094,#775,.T.);
#1278=EDGE_CURVE('',#1094,#1094,#968,.T.);
#1279=EDGE_CURVE('',#1094,#1095,#776,.T.);
#1280=EDGE_CURVE('',#1096,#1096,#969,.T.);
#1281=EDGE_CURVE('',#1096,#1097,#777,.T.);
#1282=EDGE_CURVE('',#1097,#1097,#970,.T.);
#1283=EDGE_CURVE('',#1098,#1098,#971,.T.);
#1284=EDGE_CURVE('',#1099,#1099,#972,.T.);
#1285=EDGE_CURVE('',#1100,#1100,#973,.T.);
#1286=EDGE_CURVE('',#1100,#1099,#778,.T.);
#1287=EDGE_CURVE('',#1101,#1101,#974,.T.);
#1288=EDGE_CURVE('',#1102,#1102,#975,.T.);
#1289=EDGE_CURVE('',#1101,#1103,#779,.T.);
#1290=EDGE_CURVE('',#1103,#1103,#976,.T.);
#1291=EDGE_CURVE('',#1098,#1102,#780,.T.);
#1292=EDGE_CURVE('',#1104,#1104,#977,.T.);
#1293=EDGE_CURVE('',#1104,#1105,#781,.T.);
#1294=EDGE_CURVE('',#1105,#1105,#978,.T.);
#1295=EDGE_CURVE('',#1106,#1106,#979,.T.);
#1296=EDGE_CURVE('',#1106,#1107,#782,.T.);
#1297=EDGE_CURVE('',#1107,#1107,#980,.T.);
#1298=EDGE_CURVE('',#1108,#1108,#981,.T.);
#1299=EDGE_CURVE('',#1108,#1109,#783,.T.);
#1300=EDGE_CURVE('',#1109,#1109,#982,.T.);
#1301=EDGE_CURVE('',#1110,#1110,#983,.T.);
#1302=EDGE_CURVE('',#1110,#1111,#784,.T.);
#1303=EDGE_CURVE('',#1111,#1111,#984,.T.);
#1304=EDGE_CURVE('',#1112,#1113,#785,.T.);
#1305=EDGE_CURVE('',#1114,#1112,#786,.T.);
#1306=EDGE_CURVE('',#1115,#1114,#787,.T.);
#1307=EDGE_CURVE('',#1113,#1115,#788,.T.);
#1308=EDGE_CURVE('',#1116,#1117,#789,.T.);
#1309=EDGE_CURVE('',#1118,#1116,#790,.T.);
#1310=EDGE_CURVE('',#1119,#1118,#791,.T.);
#1311=EDGE_CURVE('',#1117,#1119,#792,.T.);
#1312=EDGE_CURVE('',#1114,#1119,#985,.T.);
#1313=EDGE_CURVE('',#1117,#1112,#986,.T.);
#1314=EDGE_CURVE('',#1116,#1113,#987,.T.);
#1315=EDGE_CURVE('',#1115,#1118,#988,.T.);
#1316=ORIENTED_EDGE('',*,*,#1120,.F.);
#1317=ORIENTED_EDGE('',*,*,#1121,.T.);
#1318=ORIENTED_EDGE('',*,*,#1122,.F.);
#1319=ORIENTED_EDGE('',*,*,#1121,.F.);
#1320=ORIENTED_EDGE('',*,*,#1123,.F.);
#1321=ORIENTED_EDGE('',*,*,#1124,.T.);
#1322=ORIENTED_EDGE('',*,*,#1125,.F.);
#1323=ORIENTED_EDGE('',*,*,#1124,.F.);
#1324=ORIENTED_EDGE('',*,*,#1126,.F.);
#1325=ORIENTED_EDGE('',*,*,#1127,.T.);
#1326=ORIENTED_EDGE('',*,*,#1128,.F.);
#1327=ORIENTED_EDGE('',*,*,#1127,.F.);
#1328=ORIENTED_EDGE('',*,*,#1129,.F.);
#1329=ORIENTED_EDGE('',*,*,#1130,.T.);
#1330=ORIENTED_EDGE('',*,*,#1131,.F.);
#1331=ORIENTED_EDGE('',*,*,#1130,.F.);
#1332=ORIENTED_EDGE('',*,*,#1132,.F.);
#1333=ORIENTED_EDGE('',*,*,#1133,.T.);
#1334=ORIENTED_EDGE('',*,*,#1134,.F.);
#1335=ORIENTED_EDGE('',*,*,#1133,.F.);
#1336=ORIENTED_EDGE('',*,*,#1135,.T.);
#1337=ORIENTED_EDGE('',*,*,#1136,.T.);
#1338=ORIENTED_EDGE('',*,*,#1137,.F.);
#1339=ORIENTED_EDGE('',*,*,#1138,.F.);
#1340=ORIENTED_EDGE('',*,*,#1139,.T.);
#1341=ORIENTED_EDGE('',*,*,#1138,.T.);
#1342=ORIENTED_EDGE('',*,*,#1140,.F.);
#1343=ORIENTED_EDGE('',*,*,#1141,.F.);
#1344=ORIENTED_EDGE('',*,*,#1142,.T.);
#1345=ORIENTED_EDGE('',*,*,#1141,.T.);
#1346=ORIENTED_EDGE('',*,*,#1143,.F.);
#1347=ORIENTED_EDGE('',*,*,#1144,.F.);
#1348=ORIENTED_EDGE('',*,*,#1145,.T.);
#1349=ORIENTED_EDGE('',*,*,#1144,.T.);
#1350=ORIENTED_EDGE('',*,*,#1146,.F.);
#1351=ORIENTED_EDGE('',*,*,#1136,.F.);
#1352=ORIENTED_EDGE('',*,*,#1146,.T.);
#1353=ORIENTED_EDGE('',*,*,#1143,.T.);
#1354=ORIENTED_EDGE('',*,*,#1140,.T.);
#1355=ORIENTED_EDGE('',*,*,#1137,.T.);
#1356=ORIENTED_EDGE('',*,*,#1132,.T.);
#1357=ORIENTED_EDGE('',*,*,#1129,.T.);
#1358=ORIENTED_EDGE('',*,*,#1126,.T.);
#1359=ORIENTED_EDGE('',*,*,#1123,.T.);
#1360=ORIENTED_EDGE('',*,*,#1120,.T.);
#1361=ORIENTED_EDGE('',*,*,#1145,.F.);
#1362=ORIENTED_EDGE('',*,*,#1135,.F.);
#1363=ORIENTED_EDGE('',*,*,#1139,.F.);
#1364=ORIENTED_EDGE('',*,*,#1142,.F.);
#1365=ORIENTED_EDGE('',*,*,#1134,.T.);
#1366=ORIENTED_EDGE('',*,*,#1131,.T.);
#1367=ORIENTED_EDGE('',*,*,#1128,.T.);
#1368=ORIENTED_EDGE('',*,*,#1125,.T.);
#1369=ORIENTED_EDGE('',*,*,#1122,.T.);
#1370=ORIENTED_EDGE('',*,*,#1147,.F.);
#1371=ORIENTED_EDGE('',*,*,#1148,.T.);
#1372=ORIENTED_EDGE('',*,*,#1149,.T.);
#1373=ORIENTED_EDGE('',*,*,#1148,.F.);
#1374=ORIENTED_EDGE('',*,*,#1150,.F.);
#1375=ORIENTED_EDGE('',*,*,#1151,.T.);
#1376=ORIENTED_EDGE('',*,*,#1152,.T.);
#1377=ORIENTED_EDGE('',*,*,#1151,.F.);
#1378=ORIENTED_EDGE('',*,*,#1150,.T.);
#1379=ORIENTED_EDGE('',*,*,#1147,.T.);
#1380=ORIENTED_EDGE('',*,*,#1152,.F.);
#1381=ORIENTED_EDGE('',*,*,#1149,.F.);
#1382=ORIENTED_EDGE('',*,*,#1153,.F.);
#1383=ORIENTED_EDGE('',*,*,#1154,.T.);
#1384=ORIENTED_EDGE('',*,*,#1155,.F.);
#1385=ORIENTED_EDGE('',*,*,#1154,.F.);
#1386=ORIENTED_EDGE('',*,*,#1156,.T.);
#1387=ORIENTED_EDGE('',*,*,#1157,.T.);
#1388=ORIENTED_EDGE('',*,*,#1158,.F.);
#1389=ORIENTED_EDGE('',*,*,#1159,.F.);
#1390=ORIENTED_EDGE('',*,*,#1160,.T.);
#1391=ORIENTED_EDGE('',*,*,#1159,.T.);
#1392=ORIENTED_EDGE('',*,*,#1161,.F.);
#1393=ORIENTED_EDGE('',*,*,#1162,.F.);
#1394=ORIENTED_EDGE('',*,*,#1163,.T.);
#1395=ORIENTED_EDGE('',*,*,#1162,.T.);
#1396=ORIENTED_EDGE('',*,*,#1164,.F.);
#1397=ORIENTED_EDGE('',*,*,#1165,.F.);
#1398=ORIENTED_EDGE('',*,*,#1166,.T.);
#1399=ORIENTED_EDGE('',*,*,#1165,.T.);
#1400=ORIENTED_EDGE('',*,*,#1167,.F.);
#1401=ORIENTED_EDGE('',*,*,#1157,.F.);
#1402=ORIENTED_EDGE('',*,*,#1167,.T.);
#1403=ORIENTED_EDGE('',*,*,#1164,.T.);
#1404=ORIENTED_EDGE('',*,*,#1161,.T.);
#1405=ORIENTED_EDGE('',*,*,#1158,.T.);
#1406=ORIENTED_EDGE('',*,*,#1153,.T.);
#1407=ORIENTED_EDGE('',*,*,#1166,.F.);
#1408=ORIENTED_EDGE('',*,*,#1156,.F.);
#1409=ORIENTED_EDGE('',*,*,#1160,.F.);
#1410=ORIENTED_EDGE('',*,*,#1163,.F.);
#1411=ORIENTED_EDGE('',*,*,#1155,.T.);
#1412=ORIENTED_EDGE('',*,*,#1168,.F.);
#1413=ORIENTED_EDGE('',*,*,#1169,.T.);
#1414=ORIENTED_EDGE('',*,*,#1170,.F.);
#1415=ORIENTED_EDGE('',*,*,#1169,.F.);
#1416=ORIENTED_EDGE('',*,*,#1171,.F.);
#1417=ORIENTED_EDGE('',*,*,#1172,.T.);
#1418=ORIENTED_EDGE('',*,*,#1173,.F.);
#1419=ORIENTED_EDGE('',*,*,#1172,.F.);
#1420=ORIENTED_EDGE('',*,*,#1174,.T.);
#1421=ORIENTED_EDGE('',*,*,#1175,.T.);
#1422=ORIENTED_EDGE('',*,*,#1176,.F.);
#1423=ORIENTED_EDGE('',*,*,#1177,.F.);
#1424=ORIENTED_EDGE('',*,*,#1178,.T.);
#1425=ORIENTED_EDGE('',*,*,#1177,.T.);
#1426=ORIENTED_EDGE('',*,*,#1179,.F.);
#1427=ORIENTED_EDGE('',*,*,#1180,.F.);
#1428=ORIENTED_EDGE('',*,*,#1181,.T.);
#1429=ORIENTED_EDGE('',*,*,#1180,.T.);
#1430=ORIENTED_EDGE('',*,*,#1182,.F.);
#1431=ORIENTED_EDGE('',*,*,#1183,.F.);
#1432=ORIENTED_EDGE('',*,*,#1184,.T.);
#1433=ORIENTED_EDGE('',*,*,#1183,.T.);
#1434=ORIENTED_EDGE('',*,*,#1185,.F.);
#1435=ORIENTED_EDGE('',*,*,#1175,.F.);
#1436=ORIENTED_EDGE('',*,*,#1185,.T.);
#1437=ORIENTED_EDGE('',*,*,#1182,.T.);
#1438=ORIENTED_EDGE('',*,*,#1179,.T.);
#1439=ORIENTED_EDGE('',*,*,#1176,.T.);
#1440=ORIENTED_EDGE('',*,*,#1168,.T.);
#1441=ORIENTED_EDGE('',*,*,#1171,.T.);
#1442=ORIENTED_EDGE('',*,*,#1184,.F.);
#1443=ORIENTED_EDGE('',*,*,#1174,.F.);
#1444=ORIENTED_EDGE('',*,*,#1178,.F.);
#1445=ORIENTED_EDGE('',*,*,#1181,.F.);
#1446=ORIENTED_EDGE('',*,*,#1170,.T.);
#1447=ORIENTED_EDGE('',*,*,#1173,.T.);
#1448=ORIENTED_EDGE('',*,*,#1186,.F.);
#1449=ORIENTED_EDGE('',*,*,#1187,.T.);
#1450=ORIENTED_EDGE('',*,*,#1188,.T.);
#1451=ORIENTED_EDGE('',*,*,#1187,.F.);
#1452=ORIENTED_EDGE('',*,*,#1186,.T.);
#1453=ORIENTED_EDGE('',*,*,#1188,.F.);
#1454=ORIENTED_EDGE('',*,*,#1189,.F.);
#1455=ORIENTED_EDGE('',*,*,#1190,.T.);
#1456=ORIENTED_EDGE('',*,*,#1191,.F.);
#1457=ORIENTED_EDGE('',*,*,#1190,.F.);
#1458=ORIENTED_EDGE('',*,*,#1192,.F.);
#1459=ORIENTED_EDGE('',*,*,#1193,.T.);
#1460=ORIENTED_EDGE('',*,*,#1194,.F.);
#1461=ORIENTED_EDGE('',*,*,#1193,.F.);
#1462=ORIENTED_EDGE('',*,*,#1195,.T.);
#1463=ORIENTED_EDGE('',*,*,#1196,.T.);
#1464=ORIENTED_EDGE('',*,*,#1197,.F.);
#1465=ORIENTED_EDGE('',*,*,#1198,.F.);
#1466=ORIENTED_EDGE('',*,*,#1199,.T.);
#1467=ORIENTED_EDGE('',*,*,#1198,.T.);
#1468=ORIENTED_EDGE('',*,*,#1200,.F.);
#1469=ORIENTED_EDGE('',*,*,#1201,.F.);
#1470=ORIENTED_EDGE('',*,*,#1202,.T.);
#1471=ORIENTED_EDGE('',*,*,#1201,.T.);
#1472=ORIENTED_EDGE('',*,*,#1203,.F.);
#1473=ORIENTED_EDGE('',*,*,#1204,.F.);
#1474=ORIENTED_EDGE('',*,*,#1205,.T.);
#1475=ORIENTED_EDGE('',*,*,#1204,.T.);
#1476=ORIENTED_EDGE('',*,*,#1206,.F.);
#1477=ORIENTED_EDGE('',*,*,#1196,.F.);
#1478=ORIENTED_EDGE('',*,*,#1206,.T.);
#1479=ORIENTED_EDGE('',*,*,#1203,.T.);
#1480=ORIENTED_EDGE('',*,*,#1200,.T.);
#1481=ORIENTED_EDGE('',*,*,#1197,.T.);
#1482=ORIENTED_EDGE('',*,*,#1189,.T.);
#1483=ORIENTED_EDGE('',*,*,#1192,.T.);
#1484=ORIENTED_EDGE('',*,*,#1205,.F.);
#1485=ORIENTED_EDGE('',*,*,#1195,.F.);
#1486=ORIENTED_EDGE('',*,*,#1199,.F.);
#1487=ORIENTED_EDGE('',*,*,#1202,.F.);
#1488=ORIENTED_EDGE('',*,*,#1191,.T.);
#1489=ORIENTED_EDGE('',*,*,#1194,.T.);
#1490=ORIENTED_EDGE('',*,*,#1207,.F.);
#1491=ORIENTED_EDGE('',*,*,#1208,.T.);
#1492=ORIENTED_EDGE('',*,*,#1209,.F.);
#1493=ORIENTED_EDGE('',*,*,#1208,.F.);
#1494=ORIENTED_EDGE('',*,*,#1210,.F.);
#1495=ORIENTED_EDGE('',*,*,#1211,.T.);
#1496=ORIENTED_EDGE('',*,*,#1212,.F.);
#1497=ORIENTED_EDGE('',*,*,#1211,.F.);
#1498=ORIENTED_EDGE('',*,*,#1213,.T.);
#1499=ORIENTED_EDGE('',*,*,#1214,.T.);
#1500=ORIENTED_EDGE('',*,*,#1215,.F.);
#1501=ORIENTED_EDGE('',*,*,#1216,.F.);
#1502=ORIENTED_EDGE('',*,*,#1217,.T.);
#1503=ORIENTED_EDGE('',*,*,#1216,.T.);
#1504=ORIENTED_EDGE('',*,*,#1218,.F.);
#1505=ORIENTED_EDGE('',*,*,#1219,.F.);
#1506=ORIENTED_EDGE('',*,*,#1220,.T.);
#1507=ORIENTED_EDGE('',*,*,#1219,.T.);
#1508=ORIENTED_EDGE('',*,*,#1221,.F.);
#1509=ORIENTED_EDGE('',*,*,#1222,.F.);
#1510=ORIENTED_EDGE('',*,*,#1223,.T.);
#1511=ORIENTED_EDGE('',*,*,#1222,.T.);
#1512=ORIENTED_EDGE('',*,*,#1224,.F.);
#1513=ORIENTED_EDGE('',*,*,#1214,.F.);
#1514=ORIENTED_EDGE('',*,*,#1224,.T.);
#1515=ORIENTED_EDGE('',*,*,#1221,.T.);
#1516=ORIENTED_EDGE('',*,*,#1218,.T.);
#1517=ORIENTED_EDGE('',*,*,#1215,.T.);
#1518=ORIENTED_EDGE('',*,*,#1207,.T.);
#1519=ORIENTED_EDGE('',*,*,#1210,.T.);
#1520=ORIENTED_EDGE('',*,*,#1223,.F.);
#1521=ORIENTED_EDGE('',*,*,#1213,.F.);
#1522=ORIENTED_EDGE('',*,*,#1217,.F.);
#1523=ORIENTED_EDGE('',*,*,#1220,.F.);
#1524=ORIENTED_EDGE('',*,*,#1209,.T.);
#1525=ORIENTED_EDGE('',*,*,#1212,.T.);
#1526=ORIENTED_EDGE('',*,*,#1225,.T.);
#1527=ORIENTED_EDGE('',*,*,#1226,.T.);
#1528=ORIENTED_EDGE('',*,*,#1227,.F.);
#1529=ORIENTED_EDGE('',*,*,#1226,.F.);
#1530=ORIENTED_EDGE('',*,*,#1228,.F.);
#1531=ORIENTED_EDGE('',*,*,#1225,.F.);
#1532=ORIENTED_EDGE('',*,*,#1229,.F.);
#1533=ORIENTED_EDGE('',*,*,#1227,.T.);
#1534=ORIENTED_EDGE('',*,*,#1230,.F.);
#1535=ORIENTED_EDGE('',*,*,#1231,.T.);
#1536=ORIENTED_EDGE('',*,*,#1229,.T.);
#1537=ORIENTED_EDGE('',*,*,#1231,.F.);
#1538=ORIENTED_EDGE('',*,*,#1232,.T.);
#1539=ORIENTED_EDGE('',*,*,#1233,.F.);
#1540=ORIENTED_EDGE('',*,*,#1232,.F.);
#1541=ORIENTED_EDGE('',*,*,#1234,.T.);
#1542=ORIENTED_EDGE('',*,*,#1235,.T.);
#1543=ORIENTED_EDGE('',*,*,#1234,.F.);
#1544=ORIENTED_EDGE('',*,*,#1235,.F.);
#1545=ORIENTED_EDGE('',*,*,#1228,.T.);
#1546=ORIENTED_EDGE('',*,*,#1236,.T.);
#1547=ORIENTED_EDGE('',*,*,#1233,.T.);
#1548=ORIENTED_EDGE('',*,*,#1236,.F.);
#1549=ORIENTED_EDGE('',*,*,#1230,.T.);
#1550=ORIENTED_EDGE('',*,*,#1237,.T.);
#1551=ORIENTED_EDGE('',*,*,#1238,.T.);
#1552=ORIENTED_EDGE('',*,*,#1239,.F.);
#1553=ORIENTED_EDGE('',*,*,#1238,.F.);
#1554=ORIENTED_EDGE('',*,*,#1240,.F.);
#1555=ORIENTED_EDGE('',*,*,#1237,.F.);
#1556=ORIENTED_EDGE('',*,*,#1241,.F.);
#1557=ORIENTED_EDGE('',*,*,#1239,.T.);
#1558=ORIENTED_EDGE('',*,*,#1242,.F.);
#1559=ORIENTED_EDGE('',*,*,#1243,.T.);
#1560=ORIENTED_EDGE('',*,*,#1241,.T.);
#1561=ORIENTED_EDGE('',*,*,#1243,.F.);
#1562=ORIENTED_EDGE('',*,*,#1244,.T.);
#1563=ORIENTED_EDGE('',*,*,#1245,.F.);
#1564=ORIENTED_EDGE('',*,*,#1244,.F.);
#1565=ORIENTED_EDGE('',*,*,#1246,.T.);
#1566=ORIENTED_EDGE('',*,*,#1247,.T.);
#1567=ORIENTED_EDGE('',*,*,#1246,.F.);
#1568=ORIENTED_EDGE('',*,*,#1247,.F.);
#1569=ORIENTED_EDGE('',*,*,#1240,.T.);
#1570=ORIENTED_EDGE('',*,*,#1248,.T.);
#1571=ORIENTED_EDGE('',*,*,#1245,.T.);
#1572=ORIENTED_EDGE('',*,*,#1248,.F.);
#1573=ORIENTED_EDGE('',*,*,#1242,.T.);
#1574=ORIENTED_EDGE('',*,*,#1249,.F.);
#1575=ORIENTED_EDGE('',*,*,#1250,.T.);
#1576=ORIENTED_EDGE('',*,*,#1251,.T.);
#1577=ORIENTED_EDGE('',*,*,#1250,.F.);
#1578=ORIENTED_EDGE('',*,*,#1252,.F.);
#1579=ORIENTED_EDGE('',*,*,#1253,.T.);
#1580=ORIENTED_EDGE('',*,*,#1254,.T.);
#1581=ORIENTED_EDGE('',*,*,#1253,.F.);
#1582=ORIENTED_EDGE('',*,*,#1252,.T.);
#1583=ORIENTED_EDGE('',*,*,#1249,.T.);
#1584=ORIENTED_EDGE('',*,*,#1254,.F.);
#1585=ORIENTED_EDGE('',*,*,#1251,.F.);
#1586=ORIENTED_EDGE('',*,*,#1255,.T.);
#1587=ORIENTED_EDGE('',*,*,#1256,.T.);
#1588=ORIENTED_EDGE('',*,*,#1257,.F.);
#1589=ORIENTED_EDGE('',*,*,#1256,.F.);
#1590=ORIENTED_EDGE('',*,*,#1258,.F.);
#1591=ORIENTED_EDGE('',*,*,#1255,.F.);
#1592=ORIENTED_EDGE('',*,*,#1259,.F.);
#1593=ORIENTED_EDGE('',*,*,#1257,.T.);
#1594=ORIENTED_EDGE('',*,*,#1260,.F.);
#1595=ORIENTED_EDGE('',*,*,#1261,.T.);
#1596=ORIENTED_EDGE('',*,*,#1259,.T.);
#1597=ORIENTED_EDGE('',*,*,#1261,.F.);
#1598=ORIENTED_EDGE('',*,*,#1262,.T.);
#1599=ORIENTED_EDGE('',*,*,#1263,.F.);
#1600=ORIENTED_EDGE('',*,*,#1262,.F.);
#1601=ORIENTED_EDGE('',*,*,#1264,.T.);
#1602=ORIENTED_EDGE('',*,*,#1265,.T.);
#1603=ORIENTED_EDGE('',*,*,#1264,.F.);
#1604=ORIENTED_EDGE('',*,*,#1265,.F.);
#1605=ORIENTED_EDGE('',*,*,#1266,.F.);
#1606=ORIENTED_EDGE('',*,*,#1267,.F.);
#1607=ORIENTED_EDGE('',*,*,#1268,.T.);
#1608=ORIENTED_EDGE('',*,*,#1266,.T.);
#1609=ORIENTED_EDGE('',*,*,#1268,.F.);
#1610=ORIENTED_EDGE('',*,*,#1258,.T.);
#1611=ORIENTED_EDGE('',*,*,#1269,.T.);
#1612=ORIENTED_EDGE('',*,*,#1263,.T.);
#1613=ORIENTED_EDGE('',*,*,#1269,.F.);
#1614=ORIENTED_EDGE('',*,*,#1260,.T.);
#1615=ORIENTED_EDGE('',*,*,#1267,.T.);
#1616=ORIENTED_EDGE('',*,*,#1270,.F.);
#1617=ORIENTED_EDGE('',*,*,#1271,.T.);
#1618=ORIENTED_EDGE('',*,*,#1272,.T.);
#1619=ORIENTED_EDGE('',*,*,#1271,.F.);
#1620=ORIENTED_EDGE('',*,*,#1273,.F.);
#1621=ORIENTED_EDGE('',*,*,#1274,.T.);
#1622=ORIENTED_EDGE('',*,*,#1275,.T.);
#1623=ORIENTED_EDGE('',*,*,#1274,.F.);
#1624=ORIENTED_EDGE('',*,*,#1273,.T.);
#1625=ORIENTED_EDGE('',*,*,#1270,.T.);
#1626=ORIENTED_EDGE('',*,*,#1275,.F.);
#1627=ORIENTED_EDGE('',*,*,#1272,.F.);
#1628=ORIENTED_EDGE('',*,*,#1276,.F.);
#1629=ORIENTED_EDGE('',*,*,#1277,.T.);
#1630=ORIENTED_EDGE('',*,*,#1278,.T.);
#1631=ORIENTED_EDGE('',*,*,#1277,.F.);
#1632=ORIENTED_EDGE('',*,*,#1276,.T.);
#1633=ORIENTED_EDGE('',*,*,#1278,.F.);
#1634=ORIENTED_EDGE('',*,*,#1279,.T.);
#1635=ORIENTED_EDGE('',*,*,#1279,.F.);
#1636=ORIENTED_EDGE('',*,*,#1280,.T.);
#1637=ORIENTED_EDGE('',*,*,#1281,.T.);
#1638=ORIENTED_EDGE('',*,*,#1282,.F.);
#1639=ORIENTED_EDGE('',*,*,#1281,.F.);
#1640=ORIENTED_EDGE('',*,*,#1283,.F.);
#1641=ORIENTED_EDGE('',*,*,#1280,.F.);
#1642=ORIENTED_EDGE('',*,*,#1284,.F.);
#1643=ORIENTED_EDGE('',*,*,#1282,.T.);
#1644=ORIENTED_EDGE('',*,*,#1285,.F.);
#1645=ORIENTED_EDGE('',*,*,#1286,.T.);
#1646=ORIENTED_EDGE('',*,*,#1284,.T.);
#1647=ORIENTED_EDGE('',*,*,#1286,.F.);
#1648=ORIENTED_EDGE('',*,*,#1287,.T.);
#1649=ORIENTED_EDGE('',*,*,#1288,.F.);
#1650=ORIENTED_EDGE('',*,*,#1287,.F.);
#1651=ORIENTED_EDGE('',*,*,#1289,.T.);
#1652=ORIENTED_EDGE('',*,*,#1290,.T.);
#1653=ORIENTED_EDGE('',*,*,#1289,.F.);
#1654=ORIENTED_EDGE('',*,*,#1290,.F.);
#1655=ORIENTED_EDGE('',*,*,#1283,.T.);
#1656=ORIENTED_EDGE('',*,*,#1291,.T.);
#1657=ORIENTED_EDGE('',*,*,#1288,.T.);
#1658=ORIENTED_EDGE('',*,*,#1291,.F.);
#1659=ORIENTED_EDGE('',*,*,#1285,.T.);
#1660=ORIENTED_EDGE('',*,*,#1292,.F.);
#1661=ORIENTED_EDGE('',*,*,#1293,.T.);
#1662=ORIENTED_EDGE('',*,*,#1294,.T.);
#1663=ORIENTED_EDGE('',*,*,#1293,.F.);
#1664=ORIENTED_EDGE('',*,*,#1295,.F.);
#1665=ORIENTED_EDGE('',*,*,#1296,.T.);
#1666=ORIENTED_EDGE('',*,*,#1297,.T.);
#1667=ORIENTED_EDGE('',*,*,#1296,.F.);
#1668=ORIENTED_EDGE('',*,*,#1295,.T.);
#1669=ORIENTED_EDGE('',*,*,#1292,.T.);
#1670=ORIENTED_EDGE('',*,*,#1297,.F.);
#1671=ORIENTED_EDGE('',*,*,#1294,.F.);
#1672=ORIENTED_EDGE('',*,*,#1298,.F.);
#1673=ORIENTED_EDGE('',*,*,#1299,.T.);
#1674=ORIENTED_EDGE('',*,*,#1300,.T.);
#1675=ORIENTED_EDGE('',*,*,#1299,.F.);
#1676=ORIENTED_EDGE('',*,*,#1301,.F.);
#1677=ORIENTED_EDGE('',*,*,#1302,.T.);
#1678=ORIENTED_EDGE('',*,*,#1303,.T.);
#1679=ORIENTED_EDGE('',*,*,#1302,.F.);
#1680=ORIENTED_EDGE('',*,*,#1301,.T.);
#1681=ORIENTED_EDGE('',*,*,#1298,.T.);
#1682=ORIENTED_EDGE('',*,*,#1303,.F.);
#1683=ORIENTED_EDGE('',*,*,#1300,.F.);
#1684=ORIENTED_EDGE('',*,*,#1304,.F.);
#1685=ORIENTED_EDGE('',*,*,#1305,.F.);
#1686=ORIENTED_EDGE('',*,*,#1306,.F.);
#1687=ORIENTED_EDGE('',*,*,#1307,.F.);
#1688=ORIENTED_EDGE('',*,*,#1308,.F.);
#1689=ORIENTED_EDGE('',*,*,#1309,.F.);
#1690=ORIENTED_EDGE('',*,*,#1310,.F.);
#1691=ORIENTED_EDGE('',*,*,#1311,.F.);
#1692=ORIENTED_EDGE('',*,*,#1311,.T.);
#1693=ORIENTED_EDGE('',*,*,#1312,.F.);
#1694=ORIENTED_EDGE('',*,*,#1305,.T.);
#1695=ORIENTED_EDGE('',*,*,#1313,.F.);
#1696=ORIENTED_EDGE('',*,*,#1308,.T.);
#1697=ORIENTED_EDGE('',*,*,#1313,.T.);
#1698=ORIENTED_EDGE('',*,*,#1304,.T.);
#1699=ORIENTED_EDGE('',*,*,#1314,.F.);
#1700=ORIENTED_EDGE('',*,*,#1310,.T.);
#1701=ORIENTED_EDGE('',*,*,#1315,.F.);
#1702=ORIENTED_EDGE('',*,*,#1306,.T.);
#1703=ORIENTED_EDGE('',*,*,#1312,.T.);
#1704=ORIENTED_EDGE('',*,*,#1309,.T.);
#1705=ORIENTED_EDGE('',*,*,#1314,.T.);
#1706=ORIENTED_EDGE('',*,*,#1307,.T.);
#1707=ORIENTED_EDGE('',*,*,#1315,.T.);
#1708=CYLINDRICAL_SURFACE('',#2075,4.5);
#1709=CYLINDRICAL_SURFACE('',#2078,4.5);
#1710=CYLINDRICAL_SURFACE('',#2081,4.5);
#1711=CYLINDRICAL_SURFACE('',#2084,4.5);
#1712=CYLINDRICAL_SURFACE('',#2087,5.);
#1713=CYLINDRICAL_SURFACE('',#2097,5.);
#1714=CYLINDRICAL_SURFACE('',#2100,17.);
#1715=CYLINDRICAL_SURFACE('',#2106,5.);
#1716=CYLINDRICAL_SURFACE('',#2116,7.);
#1717=CYLINDRICAL_SURFACE('',#2119,7.);
#1718=CYLINDRICAL_SURFACE('',#2123,12.);
#1719=CYLINDRICAL_SURFACE('',#2127,12.);
#1720=CYLINDRICAL_SURFACE('',#2133,8.);
#1721=CYLINDRICAL_SURFACE('',#2139,7.);
#1722=CYLINDRICAL_SURFACE('',#2142,7.);
#1723=CYLINDRICAL_SURFACE('',#2146,12.);
#1724=CYLINDRICAL_SURFACE('',#2150,12.);
#1725=CYLINDRICAL_SURFACE('',#2156,7.);
#1726=CYLINDRICAL_SURFACE('',#2159,7.);
#1727=CYLINDRICAL_SURFACE('',#2163,12.);
#1728=CYLINDRICAL_SURFACE('',#2167,12.);
#1729=CYLINDRICAL_SURFACE('',#2173,4.);
#1730=CYLINDRICAL_SURFACE('',#2180,5.);
#1731=CYLINDRICAL_SURFACE('',#2185,8.);
#1732=CYLINDRICAL_SURFACE('',#2188,5.);
#1733=CYLINDRICAL_SURFACE('',#2191,4.);
#1734=CYLINDRICAL_SURFACE('',#2198,5.);
#1735=CYLINDRICAL_SURFACE('',#2203,8.);
#1736=CYLINDRICAL_SURFACE('',#2206,5.);
#1737=CYLINDRICAL_SURFACE('',#2209,5.);
#1738=CYLINDRICAL_SURFACE('',#2212,7.);
#1739=CYLINDRICAL_SURFACE('',#2218,4.);
#1740=CYLINDRICAL_SURFACE('',#2225,5.);
#1741=CYLINDRICAL_SURFACE('',#2230,8.);
#1742=CYLINDRICAL_SURFACE('',#2234,2.);
#1743=CYLINDRICAL_SURFACE('',#2236,5.);
#1744=CYLINDRICAL_SURFACE('',#2239,5.);
#1745=CYLINDRICAL_SURFACE('',#2242,7.);
#1746=CYLINDRICAL_SURFACE('',#2248,2.);
#1747=CYLINDRICAL_SURFACE('',#2254,4.);
#1748=CYLINDRICAL_SURFACE('',#2261,5.);
#1749=CYLINDRICAL_SURFACE('',#2266,8.);
#1750=CYLINDRICAL_SURFACE('',#2269,5.);
#1751=CYLINDRICAL_SURFACE('',#2272,5.);
#1752=CYLINDRICAL_SURFACE('',#2275,7.);
#1753=CYLINDRICAL_SURFACE('',#2281,5.);
#1754=CYLINDRICAL_SURFACE('',#2284,10.);
#1755=CYLINDRICAL_SURFACE('',#2295,4.);
#1756=CYLINDRICAL_SURFACE('',#2297,8.);
#1757=ADVANCED_FACE('',(#425),#1708,.F.);
#1758=ADVANCED_FACE('',(#426),#1709,.F.);
#1759=ADVANCED_FACE('',(#427),#1710,.F.);
#1760=ADVANCED_FACE('',(#428),#1711,.F.);
#1761=ADVANCED_FACE('',(#429),#1712,.F.);
#1762=ADVANCED_FACE('',(#430),#364,.T.);
#1763=ADVANCED_FACE('',(#431),#365,.T.);
#1764=ADVANCED_FACE('',(#432),#366,.T.);
#1765=ADVANCED_FACE('',(#433),#367,.T.);
#1766=ADVANCED_FACE('',(#434,#316,#317,#318,#319,#320),#368,.T.);
#1767=ADVANCED_FACE('',(#435,#321,#322,#323,#324,#325),#369,.F.);
#1768=ADVANCED_FACE('',(#436),#1713,.F.);
#1769=ADVANCED_FACE('',(#437),#1714,.T.);
#1770=ADVANCED_FACE('',(#438,#326),#370,.T.);
#1771=ADVANCED_FACE('',(#439,#327),#371,.F.);
#1772=ADVANCED_FACE('',(#440),#1715,.F.);
#1773=ADVANCED_FACE('',(#441),#372,.T.);
#1774=ADVANCED_FACE('',(#442),#373,.T.);
#1775=ADVANCED_FACE('',(#443),#374,.T.);
#1776=ADVANCED_FACE('',(#444),#375,.T.);
#1777=ADVANCED_FACE('',(#445,#328),#376,.T.);
#1778=ADVANCED_FACE('',(#446,#329),#377,.F.);
#1779=ADVANCED_FACE('',(#447),#1716,.F.);
#1780=ADVANCED_FACE('',(#448),#1717,.F.);
#1781=ADVANCED_FACE('',(#449),#378,.T.);
#1782=ADVANCED_FACE('',(#450),#1718,.T.);
#1783=ADVANCED_FACE('',(#451),#379,.T.);
#1784=ADVANCED_FACE('',(#452),#1719,.T.);
#1785=ADVANCED_FACE('',(#453,#330,#331),#380,.T.);
#1786=ADVANCED_FACE('',(#454,#332,#333),#381,.F.);
#1787=ADVANCED_FACE('',(#455),#1720,.T.);
#1788=ADVANCED_FACE('',(#456),#382,.T.);
#1789=ADVANCED_FACE('',(#457),#383,.F.);
#1790=ADVANCED_FACE('',(#458),#1721,.F.);
#1791=ADVANCED_FACE('',(#459),#1722,.F.);
#1792=ADVANCED_FACE('',(#460),#384,.T.);
#1793=ADVANCED_FACE('',(#461),#1723,.T.);
#1794=ADVANCED_FACE('',(#462),#385,.T.);
#1795=ADVANCED_FACE('',(#463),#1724,.T.);
#1796=ADVANCED_FACE('',(#464,#334,#335),#386,.T.);
#1797=ADVANCED_FACE('',(#465,#336,#337),#387,.F.);
#1798=ADVANCED_FACE('',(#466),#1725,.F.);
#1799=ADVANCED_FACE('',(#467),#1726,.F.);
#1800=ADVANCED_FACE('',(#468),#388,.T.);
#1801=ADVANCED_FACE('',(#469),#1727,.T.);
#1802=ADVANCED_FACE('',(#470),#389,.T.);
#1803=ADVANCED_FACE('',(#471),#1728,.T.);
#1804=ADVANCED_FACE('',(#472,#338,#339),#390,.T.);
#1805=ADVANCED_FACE('',(#473,#340,#341),#391,.F.);
#1806=ADVANCED_FACE('',(#474),#1729,.T.);
#1807=ADVANCED_FACE('',(#475,#342),#392,.F.);
#1808=ADVANCED_FACE('',(#476,#343),#393,.F.);
#1809=ADVANCED_FACE('',(#477),#1730,.T.);
#1810=ADVANCED_FACE('',(#478,#344),#394,.T.);
#1811=ADVANCED_FACE('',(#479),#1731,.T.);
#1812=ADVANCED_FACE('',(#480),#395,.F.);
#1813=ADVANCED_FACE('',(#481),#1732,.T.);
#1814=ADVANCED_FACE('',(#482),#396,.T.);
#1815=ADVANCED_FACE('',(#483),#1733,.T.);
#1816=ADVANCED_FACE('',(#484,#345),#397,.F.);
#1817=ADVANCED_FACE('',(#485,#346),#398,.F.);
#1818=ADVANCED_FACE('',(#486),#1734,.T.);
#1819=ADVANCED_FACE('',(#487,#347),#399,.T.);
#1820=ADVANCED_FACE('',(#488),#1735,.T.);
#1821=ADVANCED_FACE('',(#489),#400,.F.);
#1822=ADVANCED_FACE('',(#490),#1736,.T.);
#1823=ADVANCED_FACE('',(#491),#401,.T.);
#1824=ADVANCED_FACE('',(#492),#1737,.F.);
#1825=ADVANCED_FACE('',(#493),#1738,.T.);
#1826=ADVANCED_FACE('',(#494,#348),#402,.T.);
#1827=ADVANCED_FACE('',(#495,#349),#403,.F.);
#1828=ADVANCED_FACE('',(#496),#1739,.T.);
#1829=ADVANCED_FACE('',(#497,#350),#404,.F.);
#1830=ADVANCED_FACE('',(#498,#351),#405,.F.);
#1831=ADVANCED_FACE('',(#499),#1740,.T.);
#1832=ADVANCED_FACE('',(#500,#352),#406,.T.);
#1833=ADVANCED_FACE('',(#501),#1741,.T.);
#1834=ADVANCED_FACE('',(#502,#353),#407,.F.);
#1835=ADVANCED_FACE('',(#503),#1742,.F.);
#1836=ADVANCED_FACE('',(#504),#1743,.T.);
#1837=ADVANCED_FACE('',(#505,#354),#408,.T.);
#1838=ADVANCED_FACE('',(#506),#1744,.F.);
#1839=ADVANCED_FACE('',(#507),#1745,.T.);
#1840=ADVANCED_FACE('',(#508,#355),#409,.T.);
#1841=ADVANCED_FACE('',(#509,#356),#410,.F.);
#1842=ADVANCED_FACE('',(#510),#1746,.T.);
#1843=ADVANCED_FACE('',(#511),#411,.T.);
#1844=ADVANCED_FACE('',(#512),#247,.T.);
#1845=ADVANCED_FACE('',(#513),#1747,.T.);
#1846=ADVANCED_FACE('',(#514,#357),#412,.F.);
#1847=ADVANCED_FACE('',(#515,#358),#413,.F.);
#1848=ADVANCED_FACE('',(#516),#1748,.T.);
#1849=ADVANCED_FACE('',(#517,#359),#414,.T.);
#1850=ADVANCED_FACE('',(#518),#1749,.T.);
#1851=ADVANCED_FACE('',(#519),#415,.F.);
#1852=ADVANCED_FACE('',(#520),#1750,.T.);
#1853=ADVANCED_FACE('',(#521),#416,.T.);
#1854=ADVANCED_FACE('',(#522),#1751,.F.);
#1855=ADVANCED_FACE('',(#523),#1752,.T.);
#1856=ADVANCED_FACE('',(#524,#360),#417,.T.);
#1857=ADVANCED_FACE('',(#525,#361),#418,.F.);
#1858=ADVANCED_FACE('',(#526),#1753,.F.);
#1859=ADVANCED_FACE('',(#527),#1754,.T.);
#1860=ADVANCED_FACE('',(#528,#362),#419,.T.);
#1861=ADVANCED_FACE('',(#529,#363),#420,.F.);
#1862=ADVANCED_FACE('',(#530),#421,.F.);
#1863=ADVANCED_FACE('',(#531),#422,.F.);
#1864=ADVANCED_FACE('',(#532),#423,.F.);
#1865=ADVANCED_FACE('',(#533),#1755,.F.);
#1866=ADVANCED_FACE('',(#534),#1756,.T.);
#1867=ADVANCED_FACE('',(#535),#424,.T.);
#1868=CLOSED_SHELL('',(#1757,#1758,#1759,#1760,#1761,#1762,#1763,#1764,
#1765,#1766,#1767));
#1869=CLOSED_SHELL('',(#1768,#1769,#1770,#1771));
#1870=CLOSED_SHELL('',(#1772,#1773,#1774,#1775,#1776,#1777,#1778));
#1871=CLOSED_SHELL('',(#1779,#1780,#1781,#1782,#1783,#1784,#1785,#1786));
#1872=CLOSED_SHELL('',(#1787,#1788,#1789));
#1873=CLOSED_SHELL('',(#1790,#1791,#1792,#1793,#1794,#1795,#1796,#1797));
#1874=CLOSED_SHELL('',(#1798,#1799,#1800,#1801,#1802,#1803,#1804,#1805));
#1875=CLOSED_SHELL('',(#1806,#1807,#1808,#1809,#1810,#1811,#1812,#1813,
#1814));
#1876=CLOSED_SHELL('',(#1815,#1816,#1817,#1818,#1819,#1820,#1821,#1822,
#1823));
#1877=CLOSED_SHELL('',(#1824,#1825,#1826,#1827));
#1878=CLOSED_SHELL('',(#1828,#1829,#1830,#1831,#1832,#1833,#1834,#1835,
#1836,#1837));
#1879=CLOSED_SHELL('',(#1838,#1839,#1840,#1841));
#1880=CLOSED_SHELL('',(#1842,#1843,#1844));
#1881=CLOSED_SHELL('',(#1845,#1846,#1847,#1848,#1849,#1850,#1851,#1852,
#1853));
#1882=CLOSED_SHELL('',(#1854,#1855,#1856,#1857));
#1883=CLOSED_SHELL('',(#1858,#1859,#1860,#1861));
#1884=CLOSED_SHELL('',(#1862,#1863,#1864,#1865,#1866,#1867));
#1885=DERIVED_UNIT_ELEMENT(#1919,1.);
#1886=DERIVED_UNIT_ELEMENT(#3583,-3.);
#1887=DERIVED_UNIT_ELEMENT(#1919,1.);
#1888=DERIVED_UNIT_ELEMENT(#3583,-3.);
#1889=DERIVED_UNIT_ELEMENT(#1919,1.);
#1890=DERIVED_UNIT_ELEMENT(#3583,-3.);
#1891=DERIVED_UNIT_ELEMENT(#1919,1.);
#1892=DERIVED_UNIT_ELEMENT(#3583,-3.);
#1893=DERIVED_UNIT_ELEMENT(#1919,1.);
#1894=DERIVED_UNIT_ELEMENT(#3583,-3.);
#1895=DERIVED_UNIT_ELEMENT(#1919,1.);
#1896=DERIVED_UNIT_ELEMENT(#3583,-3.);
#1897=DERIVED_UNIT_ELEMENT(#1919,1.);
#1898=DERIVED_UNIT_ELEMENT(#3583,-3.);
#1899=DERIVED_UNIT_ELEMENT(#1919,1.);
#1900=DERIVED_UNIT_ELEMENT(#3583,-3.);
#1901=DERIVED_UNIT_ELEMENT(#1919,1.);
#1902=DERIVED_UNIT_ELEMENT(#3583,-3.);
#1903=DERIVED_UNIT_ELEMENT(#1919,1.);
#1904=DERIVED_UNIT_ELEMENT(#3583,-3.);
#1905=DERIVED_UNIT_ELEMENT(#1919,1.);
#1906=DERIVED_UNIT_ELEMENT(#3583,-3.);
#1907=DERIVED_UNIT_ELEMENT(#1919,1.);
#1908=DERIVED_UNIT_ELEMENT(#3583,-3.);
#1909=DERIVED_UNIT_ELEMENT(#1919,1.);
#1910=DERIVED_UNIT_ELEMENT(#3583,-3.);
#1911=DERIVED_UNIT_ELEMENT(#1919,1.);
#1912=DERIVED_UNIT_ELEMENT(#3583,-3.);
#1913=DERIVED_UNIT_ELEMENT(#1919,1.);
#1914=DERIVED_UNIT_ELEMENT(#3583,-3.);
#1915=DERIVED_UNIT_ELEMENT(#1919,1.);
#1916=DERIVED_UNIT_ELEMENT(#3583,-3.);
#1917=DERIVED_UNIT_ELEMENT(#1919,1.);
#1918=DERIVED_UNIT_ELEMENT(#3583,-3.);
#1919=(
MASS_UNIT()
NAMED_UNIT(*)
SI_UNIT(.KILO.,.GRAM.)
);
#1920=DERIVED_UNIT((#1885,#1886));
#1921=DERIVED_UNIT((#1887,#1888));
#1922=DERIVED_UNIT((#1889,#1890));
#1923=DERIVED_UNIT((#1891,#1892));
#1924=DERIVED_UNIT((#1893,#1894));
#1925=DERIVED_UNIT((#1895,#1896));
#1926=DERIVED_UNIT((#1897,#1898));
#1927=DERIVED_UNIT((#1899,#1900));
#1928=DERIVED_UNIT((#1901,#1902));
#1929=DERIVED_UNIT((#1903,#1904));
#1930=DERIVED_UNIT((#1905,#1906));
#1931=DERIVED_UNIT((#1907,#1908));
#1932=DERIVED_UNIT((#1909,#1910));
#1933=DERIVED_UNIT((#1911,#1912));
#1934=DERIVED_UNIT((#1913,#1914));
#1935=DERIVED_UNIT((#1915,#1916));
#1936=DERIVED_UNIT((#1917,#1918));
#1937=MEASURE_REPRESENTATION_ITEM('density measure',
POSITIVE_RATIO_MEASURE(7850.),#1920);
#1938=MEASURE_REPRESENTATION_ITEM('density measure',
POSITIVE_RATIO_MEASURE(7850.),#1921);
#1939=MEASURE_REPRESENTATION_ITEM('density measure',
POSITIVE_RATIO_MEASURE(7850.),#1922);
#1940=MEASURE_REPRESENTATION_ITEM('density measure',
POSITIVE_RATIO_MEASURE(7850.),#1923);
#1941=MEASURE_REPRESENTATION_ITEM('density measure',
POSITIVE_RATIO_MEASURE(7850.),#1924);
#1942=MEASURE_REPRESENTATION_ITEM('density measure',
POSITIVE_RATIO_MEASURE(7850.),#1925);
#1943=MEASURE_REPRESENTATION_ITEM('density measure',
POSITIVE_RATIO_MEASURE(7850.),#1926);
#1944=MEASURE_REPRESENTATION_ITEM('density measure',
POSITIVE_RATIO_MEASURE(7850.),#1927);
#1945=MEASURE_REPRESENTATION_ITEM('density measure',
POSITIVE_RATIO_MEASURE(7850.),#1928);
#1946=MEASURE_REPRESENTATION_ITEM('density measure',
POSITIVE_RATIO_MEASURE(7850.),#1929);
#1947=MEASURE_REPRESENTATION_ITEM('density measure',
POSITIVE_RATIO_MEASURE(7850.),#1930);
#1948=MEASURE_REPRESENTATION_ITEM('density measure',
POSITIVE_RATIO_MEASURE(8920.),#1931);
#1949=MEASURE_REPRESENTATION_ITEM('density measure',
POSITIVE_RATIO_MEASURE(7850.),#1932);
#1950=MEASURE_REPRESENTATION_ITEM('density measure',
POSITIVE_RATIO_MEASURE(7850.),#1933);
#1951=MEASURE_REPRESENTATION_ITEM('density measure',
POSITIVE_RATIO_MEASURE(7850.),#1934);
#1952=MEASURE_REPRESENTATION_ITEM('density measure',
POSITIVE_RATIO_MEASURE(7850.),#1935);
#1953=MEASURE_REPRESENTATION_ITEM('density measure',
POSITIVE_RATIO_MEASURE(7850.),#1936);
#1954=PROPERTY_DEFINITION_REPRESENTATION(#2039,#1988);
#1955=PROPERTY_DEFINITION_REPRESENTATION(#2040,#1989);
#1956=PROPERTY_DEFINITION_REPRESENTATION(#2041,#1990);
#1957=PROPERTY_DEFINITION_REPRESENTATION(#2042,#1991);
#1958=PROPERTY_DEFINITION_REPRESENTATION(#2043,#1992);
#1959=PROPERTY_DEFINITION_REPRESENTATION(#2044,#1993);
#1960=PROPERTY_DEFINITION_REPRESENTATION(#2045,#1994);
#1961=PROPERTY_DEFINITION_REPRESENTATION(#2046,#1995);
#1962=PROPERTY_DEFINITION_REPRESENTATION(#2047,#1996);
#1963=PROPERTY_DEFINITION_REPRESENTATION(#2048,#1997);
#1964=PROPERTY_DEFINITION_REPRESENTATION(#2049,#1998);
#1965=PROPERTY_DEFINITION_REPRESENTATION(#2050,#1999);
#1966=PROPERTY_DEFINITION_REPRESENTATION(#2051,#2000);
#1967=PROPERTY_DEFINITION_REPRESENTATION(#2052,#2001);
#1968=PROPERTY_DEFINITION_REPRESENTATION(#2053,#2002);
#1969=PROPERTY_DEFINITION_REPRESENTATION(#2054,#2003);
#1970=PROPERTY_DEFINITION_REPRESENTATION(#2055,#2004);
#1971=PROPERTY_DEFINITION_REPRESENTATION(#2056,#2005);
#1972=PROPERTY_DEFINITION_REPRESENTATION(#2057,#2006);
#1973=PROPERTY_DEFINITION_REPRESENTATION(#2058,#2007);
#1974=PROPERTY_DEFINITION_REPRESENTATION(#2059,#2008);
#1975=PROPERTY_DEFINITION_REPRESENTATION(#2060,#2009);
#1976=PROPERTY_DEFINITION_REPRESENTATION(#2061,#2010);
#1977=PROPERTY_DEFINITION_REPRESENTATION(#2062,#2011);
#1978=PROPERTY_DEFINITION_REPRESENTATION(#2063,#2012);
#1979=PROPERTY_DEFINITION_REPRESENTATION(#2064,#2013);
#1980=PROPERTY_DEFINITION_REPRESENTATION(#2065,#2014);
#1981=PROPERTY_DEFINITION_REPRESENTATION(#2066,#2015);
#1982=PROPERTY_DEFINITION_REPRESENTATION(#2067,#2016);
#1983=PROPERTY_DEFINITION_REPRESENTATION(#2068,#2017);
#1984=PROPERTY_DEFINITION_REPRESENTATION(#2069,#2018);
#1985=PROPERTY_DEFINITION_REPRESENTATION(#2070,#2019);
#1986=PROPERTY_DEFINITION_REPRESENTATION(#2071,#2020);
#1987=PROPERTY_DEFINITION_REPRESENTATION(#2072,#2021);
#1988=REPRESENTATION('material name',(#2022),#3564);
#1989=REPRESENTATION('density',(#1937),#3564);
#1990=REPRESENTATION('material name',(#2023),#3565);
#1991=REPRESENTATION('density',(#1938),#3565);
#1992=REPRESENTATION('material name',(#2024),#3566);
#1993=REPRESENTATION('density',(#1939),#3566);
#1994=REPRESENTATION('material name',(#2025),#3567);
#1995=REPRESENTATION('density',(#1940),#3567);
#1996=REPRESENTATION('material name',(#2026),#3568);
#1997=REPRESENTATION('density',(#1941),#3568);
#1998=REPRESENTATION('material name',(#2027),#3569);
#1999=REPRESENTATION('density',(#1942),#3569);
#2000=REPRESENTATION('material name',(#2028),#3570);
#2001=REPRESENTATION('density',(#1943),#3570);
#2002=REPRESENTATION('material name',(#2029),#3571);
#2003=REPRESENTATION('density',(#1944),#3571);
#2004=REPRESENTATION('material name',(#2030),#3572);
#2005=REPRESENTATION('density',(#1945),#3572);
#2006=REPRESENTATION('material name',(#2031),#3573);
#2007=REPRESENTATION('density',(#1946),#3573);
#2008=REPRESENTATION('material name',(#2032),#3574);
#2009=REPRESENTATION('density',(#1947),#3574);
#2010=REPRESENTATION('material name',(#2033),#3575);
#2011=REPRESENTATION('density',(#1948),#3575);
#2012=REPRESENTATION('material name',(#2034),#3576);
#2013=REPRESENTATION('density',(#1949),#3576);
#2014=REPRESENTATION('material name',(#2035),#3577);
#2015=REPRESENTATION('density',(#1950),#3577);
#2016=REPRESENTATION('material name',(#2036),#3578);
#2017=REPRESENTATION('density',(#1951),#3578);
#2018=REPRESENTATION('material name',(#2037),#3579);
#2019=REPRESENTATION('density',(#1952),#3579);
#2020=REPRESENTATION('material name',(#2038),#3580);
#2021=REPRESENTATION('density',(#1953),#3580);
#2022=DESCRIPTIVE_REPRESENTATION_ITEM('Steel','Steel');
#2023=DESCRIPTIVE_REPRESENTATION_ITEM('Steel','Steel');
#2024=DESCRIPTIVE_REPRESENTATION_ITEM('Steel','Steel');
#2025=DESCRIPTIVE_REPRESENTATION_ITEM('Steel','Steel');
#2026=DESCRIPTIVE_REPRESENTATION_ITEM('Steel','Steel');
#2027=DESCRIPTIVE_REPRESENTATION_ITEM('Steel','Steel');
#2028=DESCRIPTIVE_REPRESENTATION_ITEM('Steel','Steel');
#2029=DESCRIPTIVE_REPRESENTATION_ITEM('Steel','Steel');
#2030=DESCRIPTIVE_REPRESENTATION_ITEM('Steel','Steel');
#2031=DESCRIPTIVE_REPRESENTATION_ITEM('Steel','Steel');
#2032=DESCRIPTIVE_REPRESENTATION_ITEM('Steel','Steel');
#2033=DESCRIPTIVE_REPRESENTATION_ITEM('Copper, Alloy','Copper, Alloy');
#2034=DESCRIPTIVE_REPRESENTATION_ITEM('Steel','Steel');
#2035=DESCRIPTIVE_REPRESENTATION_ITEM('Steel','Steel');
#2036=DESCRIPTIVE_REPRESENTATION_ITEM('Steel','Steel');
#2037=DESCRIPTIVE_REPRESENTATION_ITEM('Steel','Steel');
#2038=DESCRIPTIVE_REPRESENTATION_ITEM('Steel','Steel');
#2039=PROPERTY_DEFINITION('material property','material name',#3701);
#2040=PROPERTY_DEFINITION('material property','density of part',#3701);
#2041=PROPERTY_DEFINITION('material property','material name',#3702);
#2042=PROPERTY_DEFINITION('material property','density of part',#3702);
#2043=PROPERTY_DEFINITION('material property','material name',#3703);
#2044=PROPERTY_DEFINITION('material property','density of part',#3703);
#2045=PROPERTY_DEFINITION('material property','material name',#3704);
#2046=PROPERTY_DEFINITION('material property','density of part',#3704);
#2047=PROPERTY_DEFINITION('material property','material name',#3705);
#2048=PROPERTY_DEFINITION('material property','density of part',#3705);
#2049=PROPERTY_DEFINITION('material property','material name',#3706);
#2050=PROPERTY_DEFINITION('material property','density of part',#3706);
#2051=PROPERTY_DEFINITION('material property','material name',#3707);
#2052=PROPERTY_DEFINITION('material property','density of part',#3707);
#2053=PROPERTY_DEFINITION('material property','material name',#3708);
#2054=PROPERTY_DEFINITION('material property','density of part',#3708);
#2055=PROPERTY_DEFINITION('material property','material name',#3709);
#2056=PROPERTY_DEFINITION('material property','density of part',#3709);
#2057=PROPERTY_DEFINITION('material property','material name',#3710);
#2058=PROPERTY_DEFINITION('material property','density of part',#3710);
#2059=PROPERTY_DEFINITION('material property','material name',#3711);
#2060=PROPERTY_DEFINITION('material property','density of part',#3711);
#2061=PROPERTY_DEFINITION('material property','material name',#3712);
#2062=PROPERTY_DEFINITION('material property','density of part',#3712);
#2063=PROPERTY_DEFINITION('material property','material name',#3713);
#2064=PROPERTY_DEFINITION('material property','density of part',#3713);
#2065=PROPERTY_DEFINITION('material property','material name',#3714);
#2066=PROPERTY_DEFINITION('material property','density of part',#3714);
#2067=PROPERTY_DEFINITION('material property','material name',#3715);
#2068=PROPERTY_DEFINITION('material property','density of part',#3715);
#2069=PROPERTY_DEFINITION('material property','material name',#3716);
#2070=PROPERTY_DEFINITION('material property','density of part',#3716);
#2071=PROPERTY_DEFINITION('material property','material name',#3717);
#2072=PROPERTY_DEFINITION('material property','density of part',#3717);
#2073=AXIS2_PLACEMENT_3D('',#3029,#2359,#2360);
#2074=AXIS2_PLACEMENT_3D('',#3030,#2361,#2362);
#2075=AXIS2_PLACEMENT_3D('',#3031,#2363,#2364);
#2076=AXIS2_PLACEMENT_3D('',#3033,#2365,#2366);
#2077=AXIS2_PLACEMENT_3D('',#3036,#2368,#2369);
#2078=AXIS2_PLACEMENT_3D('',#3037,#2370,#2371);
#2079=AXIS2_PLACEMENT_3D('',#3039,#2372,#2373);
#2080=AXIS2_PLACEMENT_3D('',#3042,#2375,#2376);
#2081=AXIS2_PLACEMENT_3D('',#3043,#2377,#2378);
#2082=AXIS2_PLACEMENT_3D('',#3045,#2379,#2380);
#2083=AXIS2_PLACEMENT_3D('',#3048,#2382,#2383);
#2084=AXIS2_PLACEMENT_3D('',#3049,#2384,#2385);
#2085=AXIS2_PLACEMENT_3D('',#3051,#2386,#2387);
#2086=AXIS2_PLACEMENT_3D('',#3054,#2389,#2390);
#2087=AXIS2_PLACEMENT_3D('',#3055,#2391,#2392);
#2088=AXIS2_PLACEMENT_3D('',#3057,#2393,#2394);
#2089=AXIS2_PLACEMENT_3D('',#3060,#2396,#2397);
#2090=AXIS2_PLACEMENT_3D('',#3061,#2398,#2399);
#2091=AXIS2_PLACEMENT_3D('',#3070,#2404,#2405);
#2092=AXIS2_PLACEMENT_3D('',#3076,#2409,#2410);
#2093=AXIS2_PLACEMENT_3D('',#3082,#2414,#2415);
#2094=AXIS2_PLACEMENT_3D('',#3085,#2418,#2419);
#2095=AXIS2_PLACEMENT_3D('',#3086,#2420,#2421);
#2096=AXIS2_PLACEMENT_3D('',#3087,#2422,#2423);
#2097=AXIS2_PLACEMENT_3D('',#3088,#2424,#2425);
#2098=AXIS2_PLACEMENT_3D('',#3090,#2426,#2427);
#2099=AXIS2_PLACEMENT_3D('',#3093,#2429,#2430);
#2100=AXIS2_PLACEMENT_3D('',#3094,#2431,#2432);
#2101=AXIS2_PLACEMENT_3D('',#3096,#2433,#2434);
#2102=AXIS2_PLACEMENT_3D('',#3099,#2436,#2437);
#2103=AXIS2_PLACEMENT_3D('',#3100,#2438,#2439);
#2104=AXIS2_PLACEMENT_3D('',#3101,#2440,#2441);
#2105=AXIS2_PLACEMENT_3D('',#3102,#2442,#2443);
#2106=AXIS2_PLACEMENT_3D('',#3103,#2444,#2445);
#2107=AXIS2_PLACEMENT_3D('',#3105,#2446,#2447);
#2108=AXIS2_PLACEMENT_3D('',#3108,#2449,#2450);
#2109=AXIS2_PLACEMENT_3D('',#3109,#2451,#2452);
#2110=AXIS2_PLACEMENT_3D('',#3118,#2457,#2458);
#2111=AXIS2_PLACEMENT_3D('',#3124,#2462,#2463);
#2112=AXIS2_PLACEMENT_3D('',#3130,#2467,#2468);
#2113=AXIS2_PLACEMENT_3D('',#3133,#2471,#2472);
#2114=AXIS2_PLACEMENT_3D('',#3134,#2473,#2474);
#2115=AXIS2_PLACEMENT_3D('',#3135,#2475,#2476);
#2116=AXIS2_PLACEMENT_3D('',#3136,#2477,#2478);
#2117=AXIS2_PLACEMENT_3D('',#3138,#2479,#2480);
#2118=AXIS2_PLACEMENT_3D('',#3141,#2482,#2483);
#2119=AXIS2_PLACEMENT_3D('',#3142,#2484,#2485);
#2120=AXIS2_PLACEMENT_3D('',#3144,#2486,#2487);
#2121=AXIS2_PLACEMENT_3D('',#3147,#2489,#2490);
#2122=AXIS2_PLACEMENT_3D('',#3148,#2491,#2492);
#2123=AXIS2_PLACEMENT_3D('',#3157,#2497,#2498);
#2124=AXIS2_PLACEMENT_3D('',#3159,#2499,#2500);
#2125=AXIS2_PLACEMENT_3D('',#3161,#2501,#2502);
#2126=AXIS2_PLACEMENT_3D('',#3163,#2504,#2505);
#2127=AXIS2_PLACEMENT_3D('',#3169,#2509,#2510);
#2128=AXIS2_PLACEMENT_3D('',#3170,#2511,#2512);
#2129=AXIS2_PLACEMENT_3D('',#3171,#2513,#2514);
#2130=AXIS2_PLACEMENT_3D('',#3172,#2515,#2516);
#2131=AXIS2_PLACEMENT_3D('',#3173,#2517,#2518);
#2132=AXIS2_PLACEMENT_3D('',#3174,#2519,#2520);
#2133=AXIS2_PLACEMENT_3D('',#3175,#2521,#2522);
#2134=AXIS2_PLACEMENT_3D('',#3177,#2523,#2524);
#2135=AXIS2_PLACEMENT_3D('',#3180,#2526,#2527);
#2136=AXIS2_PLACEMENT_3D('',#3181,#2528,#2529);
#2137=AXIS2_PLACEMENT_3D('',#3182,#2530,#2531);
#2138=AXIS2_PLACEMENT_3D('',#3183,#2532,#2533);
#2139=AXIS2_PLACEMENT_3D('',#3184,#2534,#2535);
#2140=AXIS2_PLACEMENT_3D('',#3186,#2536,#2537);
#2141=AXIS2_PLACEMENT_3D('',#3189,#2539,#2540);
#2142=AXIS2_PLACEMENT_3D('',#3190,#2541,#2542);
#2143=AXIS2_PLACEMENT_3D('',#3192,#2543,#2544);
#2144=AXIS2_PLACEMENT_3D('',#3195,#2546,#2547);
#2145=AXIS2_PLACEMENT_3D('',#3196,#2548,#2549);
#2146=AXIS2_PLACEMENT_3D('',#3205,#2554,#2555);
#2147=AXIS2_PLACEMENT_3D('',#3207,#2556,#2557);
#2148=AXIS2_PLACEMENT_3D('',#3209,#2558,#2559);
#2149=AXIS2_PLACEMENT_3D('',#3211,#2561,#2562);
#2150=AXIS2_PLACEMENT_3D('',#3217,#2566,#2567);
#2151=AXIS2_PLACEMENT_3D('',#3218,#2568,#2569);
#2152=AXIS2_PLACEMENT_3D('',#3219,#2570,#2571);
#2153=AXIS2_PLACEMENT_3D('',#3220,#2572,#2573);
#2154=AXIS2_PLACEMENT_3D('',#3221,#2574,#2575);
#2155=AXIS2_PLACEMENT_3D('',#3222,#2576,#2577);
#2156=AXIS2_PLACEMENT_3D('',#3223,#2578,#2579);
#2157=AXIS2_PLACEMENT_3D('',#3225,#2580,#2581);
#2158=AXIS2_PLACEMENT_3D('',#3228,#2583,#2584);
#2159=AXIS2_PLACEMENT_3D('',#3229,#2585,#2586);
#2160=AXIS2_PLACEMENT_3D('',#3231,#2587,#2588);
#2161=AXIS2_PLACEMENT_3D('',#3234,#2590,#2591);
#2162=AXIS2_PLACEMENT_3D('',#3235,#2592,#2593);
#2163=AXIS2_PLACEMENT_3D('',#3244,#2598,#2599);
#2164=AXIS2_PLACEMENT_3D('',#3246,#2600,#2601);
#2165=AXIS2_PLACEMENT_3D('',#3248,#2602,#2603);
#2166=AXIS2_PLACEMENT_3D('',#3250,#2605,#2606);
#2167=AXIS2_PLACEMENT_3D('',#3256,#2610,#2611);
#2168=AXIS2_PLACEMENT_3D('',#3257,#2612,#2613);
#2169=AXIS2_PLACEMENT_3D('',#3258,#2614,#2615);
#2170=AXIS2_PLACEMENT_3D('',#3259,#2616,#2617);
#2171=AXIS2_PLACEMENT_3D('',#3260,#2618,#2619);
#2172=AXIS2_PLACEMENT_3D('',#3261,#2620,#2621);
#2173=AXIS2_PLACEMENT_3D('',#3262,#2622,#2623);
#2174=AXIS2_PLACEMENT_3D('',#3264,#2624,#2625);
#2175=AXIS2_PLACEMENT_3D('',#3267,#2627,#2628);
#2176=AXIS2_PLACEMENT_3D('',#3268,#2629,#2630);
#2177=AXIS2_PLACEMENT_3D('',#3270,#2631,#2632);
#2178=AXIS2_PLACEMENT_3D('',#3271,#2633,#2634);
#2179=AXIS2_PLACEMENT_3D('',#3273,#2635,#2636);
#2180=AXIS2_PLACEMENT_3D('',#3274,#2637,#2638);
#2181=AXIS2_PLACEMENT_3D('',#3276,#2639,#2640);
#2182=AXIS2_PLACEMENT_3D('',#3278,#2642,#2643);
#2183=AXIS2_PLACEMENT_3D('',#3280,#2644,#2645);
#2184=AXIS2_PLACEMENT_3D('',#3282,#2646,#2647);
#2185=AXIS2_PLACEMENT_3D('',#3283,#2648,#2649);
#2186=AXIS2_PLACEMENT_3D('',#3286,#2651,#2652);
#2187=AXIS2_PLACEMENT_3D('',#3287,#2653,#2654);
#2188=AXIS2_PLACEMENT_3D('',#3288,#2655,#2656);
#2189=AXIS2_PLACEMENT_3D('',#3290,#2658,#2659);
#2190=AXIS2_PLACEMENT_3D('',#3291,#2660,#2661);
#2191=AXIS2_PLACEMENT_3D('',#3292,#2662,#2663);
#2192=AXIS2_PLACEMENT_3D('',#3294,#2664,#2665);
#2193=AXIS2_PLACEMENT_3D('',#3297,#2667,#2668);
#2194=AXIS2_PLACEMENT_3D('',#3298,#2669,#2670);
#2195=AXIS2_PLACEMENT_3D('',#3300,#2671,#2672);
#2196=AXIS2_PLACEMENT_3D('',#3301,#2673,#2674);
#2197=AXIS2_PLACEMENT_3D('',#3303,#2675,#2676);
#2198=AXIS2_PLACEMENT_3D('',#3304,#2677,#2678);
#2199=AXIS2_PLACEMENT_3D('',#3306,#2679,#2680);
#2200=AXIS2_PLACEMENT_3D('',#3308,#2682,#2683);
#2201=AXIS2_PLACEMENT_3D('',#3310,#2684,#2685);
#2202=AXIS2_PLACEMENT_3D('',#3312,#2686,#2687);
#2203=AXIS2_PLACEMENT_3D('',#3313,#2688,#2689);
#2204=AXIS2_PLACEMENT_3D('',#3316,#2691,#2692);
#2205=AXIS2_PLACEMENT_3D('',#3317,#2693,#2694);
#2206=AXIS2_PLACEMENT_3D('',#3318,#2695,#2696);
#2207=AXIS2_PLACEMENT_3D('',#3320,#2698,#2699);
#2208=AXIS2_PLACEMENT_3D('',#3321,#2700,#2701);
#2209=AXIS2_PLACEMENT_3D('',#3322,#2702,#2703);
#2210=AXIS2_PLACEMENT_3D('',#3324,#2704,#2705);
#2211=AXIS2_PLACEMENT_3D('',#3327,#2707,#2708);
#2212=AXIS2_PLACEMENT_3D('',#3328,#2709,#2710);
#2213=AXIS2_PLACEMENT_3D('',#3330,#2711,#2712);
#2214=AXIS2_PLACEMENT_3D('',#3333,#2714,#2715);
#2215=AXIS2_PLACEMENT_3D('',#3334,#2716,#2717);
#2216=AXIS2_PLACEMENT_3D('',#3335,#2718,#2719);
#2217=AXIS2_PLACEMENT_3D('',#3336,#2720,#2721);
#2218=AXIS2_PLACEMENT_3D('',#3337,#2722,#2723);
#2219=AXIS2_PLACEMENT_3D('',#3339,#2724,#2725);
#2220=AXIS2_PLACEMENT_3D('',#3342,#2727,#2728);
#2221=AXIS2_PLACEMENT_3D('',#3343,#2729,#2730);
#2222=AXIS2_PLACEMENT_3D('',#3345,#2731,#2732);
#2223=AXIS2_PLACEMENT_3D('',#3346,#2733,#2734);
#2224=AXIS2_PLACEMENT_3D('',#3348,#2735,#2736);
#2225=AXIS2_PLACEMENT_3D('',#3349,#2737,#2738);
#2226=AXIS2_PLACEMENT_3D('',#3351,#2739,#2740);
#2227=AXIS2_PLACEMENT_3D('',#3353,#2742,#2743);
#2228=AXIS2_PLACEMENT_3D('',#3355,#2744,#2745);
#2229=AXIS2_PLACEMENT_3D('',#3357,#2746,#2747);
#2230=AXIS2_PLACEMENT_3D('',#3358,#2748,#2749);
#2231=AXIS2_PLACEMENT_3D('',#3361,#2751,#2752);
#2232=AXIS2_PLACEMENT_3D('',#3362,#2753,#2754);
#2233=AXIS2_PLACEMENT_3D('',#3364,#2755,#2756);
#2234=AXIS2_PLACEMENT_3D('',#3365,#2757,#2758);
#2235=AXIS2_PLACEMENT_3D('',#3367,#2759,#2760);
#2236=AXIS2_PLACEMENT_3D('',#3369,#2762,#2763);
#2237=AXIS2_PLACEMENT_3D('',#3371,#2765,#2766);
#2238=AXIS2_PLACEMENT_3D('',#3372,#2767,#2768);
#2239=AXIS2_PLACEMENT_3D('',#3373,#2769,#2770);
#2240=AXIS2_PLACEMENT_3D('',#3375,#2771,#2772);
#2241=AXIS2_PLACEMENT_3D('',#3378,#2774,#2775);
#2242=AXIS2_PLACEMENT_3D('',#3379,#2776,#2777);
#2243=AXIS2_PLACEMENT_3D('',#3381,#2778,#2779);
#2244=AXIS2_PLACEMENT_3D('',#3384,#2781,#2782);
#2245=AXIS2_PLACEMENT_3D('',#3385,#2783,#2784);
#2246=AXIS2_PLACEMENT_3D('',#3386,#2785,#2786);
#2247=AXIS2_PLACEMENT_3D('',#3387,#2787,#2788);
#2248=AXIS2_PLACEMENT_3D('',#3388,#2789,#2790);
#2249=AXIS2_PLACEMENT_3D('',#3390,#2791,#2792);
#2250=AXIS2_PLACEMENT_3D('',#3393,#2794,#2795);
#2251=AXIS2_PLACEMENT_3D('',#3394,#2796,#2797);
#2252=AXIS2_PLACEMENT_3D('',#3395,#2798,#2799);
#2253=AXIS2_PLACEMENT_3D('',#3398,#2801,#2802);
#2254=AXIS2_PLACEMENT_3D('',#3399,#2803,#2804);
#2255=AXIS2_PLACEMENT_3D('',#3401,#2805,#2806);
#2256=AXIS2_PLACEMENT_3D('',#3404,#2808,#2809);
#2257=AXIS2_PLACEMENT_3D('',#3405,#2810,#2811);
#2258=AXIS2_PLACEMENT_3D('',#3407,#2812,#2813);
#2259=AXIS2_PLACEMENT_3D('',#3408,#2814,#2815);
#2260=AXIS2_PLACEMENT_3D('',#3410,#2816,#2817);
#2261=AXIS2_PLACEMENT_3D('',#3411,#2818,#2819);
#2262=AXIS2_PLACEMENT_3D('',#3413,#2820,#2821);
#2263=AXIS2_PLACEMENT_3D('',#3415,#2823,#2824);
#2264=AXIS2_PLACEMENT_3D('',#3417,#2825,#2826);
#2265=AXIS2_PLACEMENT_3D('',#3419,#2827,#2828);
#2266=AXIS2_PLACEMENT_3D('',#3420,#2829,#2830);
#2267=AXIS2_PLACEMENT_3D('',#3423,#2832,#2833);
#2268=AXIS2_PLACEMENT_3D('',#3424,#2834,#2835);
#2269=AXIS2_PLACEMENT_3D('',#3425,#2836,#2837);
#2270=AXIS2_PLACEMENT_3D('',#3427,#2839,#2840);
#2271=AXIS2_PLACEMENT_3D('',#3428,#2841,#2842);
#2272=AXIS2_PLACEMENT_3D('',#3429,#2843,#2844);
#2273=AXIS2_PLACEMENT_3D('',#3431,#2845,#2846);
#2274=AXIS2_PLACEMENT_3D('',#3434,#2848,#2849);
#2275=AXIS2_PLACEMENT_3D('',#3435,#2850,#2851);
#2276=AXIS2_PLACEMENT_3D('',#3437,#2852,#2853);
#2277=AXIS2_PLACEMENT_3D('',#3440,#2855,#2856);
#2278=AXIS2_PLACEMENT_3D('',#3441,#2857,#2858);
#2279=AXIS2_PLACEMENT_3D('',#3442,#2859,#2860);
#2280=AXIS2_PLACEMENT_3D('',#3443,#2861,#2862);
#2281=AXIS2_PLACEMENT_3D('',#3444,#2863,#2864);
#2282=AXIS2_PLACEMENT_3D('',#3446,#2865,#2866);
#2283=AXIS2_PLACEMENT_3D('',#3449,#2868,#2869);
#2284=AXIS2_PLACEMENT_3D('',#3450,#2870,#2871);
#2285=AXIS2_PLACEMENT_3D('',#3452,#2872,#2873);
#2286=AXIS2_PLACEMENT_3D('',#3455,#2875,#2876);
#2287=AXIS2_PLACEMENT_3D('',#3456,#2877,#2878);
#2288=AXIS2_PLACEMENT_3D('',#3457,#2879,#2880);
#2289=AXIS2_PLACEMENT_3D('',#3458,#2881,#2882);
#2290=AXIS2_PLACEMENT_3D('',#3459,#2883,#2884);
#2291=AXIS2_PLACEMENT_3D('',#3468,#2889,#2890);
#2292=AXIS2_PLACEMENT_3D('',#3477,#2895,#2896);
#2293=AXIS2_PLACEMENT_3D('',#3478,#2897,#2898);
#2294=AXIS2_PLACEMENT_3D('',#3479,#2899,#2900);
#2295=AXIS2_PLACEMENT_3D('',#3480,#2901,#2902);
#2296=AXIS2_PLACEMENT_3D('',#3481,#2903,#2904);
#2297=AXIS2_PLACEMENT_3D('',#3482,#2905,#2906);
#2298=AXIS2_PLACEMENT_3D('',#3483,#2907,#2908);
#2299=AXIS2_PLACEMENT_3D('',#3484,#2909,#2910);
#2300=AXIS2_PLACEMENT_3D('',#3485,#2911,#2912);
#2301=AXIS2_PLACEMENT_3D('',#3486,#2913,#2914);
#2302=AXIS2_PLACEMENT_3D('',#3487,#2915,#2916);
#2303=AXIS2_PLACEMENT_3D('',#3488,#2917,#2918);
#2304=AXIS2_PLACEMENT_3D('',#3489,#2919,#2920);
#2305=AXIS2_PLACEMENT_3D('',#3490,#2921,#2922);
#2306=AXIS2_PLACEMENT_3D('',#3491,#2923,#2924);
#2307=AXIS2_PLACEMENT_3D('',#3492,#2925,#2926);
#2308=AXIS2_PLACEMENT_3D('',#3493,#2927,#2928);
#2309=AXIS2_PLACEMENT_3D('',#3494,#2929,#2930);
#2310=AXIS2_PLACEMENT_3D('',#3495,#2931,#2932);
#2311=AXIS2_PLACEMENT_3D('',#3496,#2933,#2934);
#2312=AXIS2_PLACEMENT_3D('',#3497,#2935,#2936);
#2313=AXIS2_PLACEMENT_3D('',#3498,#2937,#2938);
#2314=AXIS2_PLACEMENT_3D('',#3499,#2939,#2940);
#2315=AXIS2_PLACEMENT_3D('',#3500,#2941,#2942);
#2316=AXIS2_PLACEMENT_3D('',#3501,#2943,#2944);
#2317=AXIS2_PLACEMENT_3D('',#3502,#2945,#2946);
#2318=AXIS2_PLACEMENT_3D('',#3503,#2947,#2948);
#2319=AXIS2_PLACEMENT_3D('',#3504,#2949,#2950);
#2320=AXIS2_PLACEMENT_3D('',#3505,#2951,#2952);
#2321=AXIS2_PLACEMENT_3D('',#3506,#2953,#2954);
#2322=AXIS2_PLACEMENT_3D('',#3507,#2955,#2956);
#2323=AXIS2_PLACEMENT_3D('',#3508,#2957,#2958);
#2324=AXIS2_PLACEMENT_3D('',#3509,#2959,#2960);
#2325=AXIS2_PLACEMENT_3D('',#3510,#2961,#2962);
#2326=AXIS2_PLACEMENT_3D('',#3511,#2963,#2964);
#2327=AXIS2_PLACEMENT_3D('',#3512,#2965,#2966);
#2328=AXIS2_PLACEMENT_3D('',#3513,#2967,#2968);
#2329=AXIS2_PLACEMENT_3D('',#3514,#2969,#2970);
#2330=AXIS2_PLACEMENT_3D('',#3515,#2971,#2972);
#2331=AXIS2_PLACEMENT_3D('',#3516,#2973,#2974);
#2332=AXIS2_PLACEMENT_3D('',#3517,#2975,#2976);
#2333=AXIS2_PLACEMENT_3D('',#3518,#2977,#2978);
#2334=AXIS2_PLACEMENT_3D('',#3519,#2979,#2980);
#2335=AXIS2_PLACEMENT_3D('',#3520,#2981,#2982);
#2336=AXIS2_PLACEMENT_3D('',#3521,#2983,#2984);
#2337=AXIS2_PLACEMENT_3D('',#3522,#2985,#2986);
#2338=AXIS2_PLACEMENT_3D('',#3523,#2987,#2988);
#2339=AXIS2_PLACEMENT_3D('',#3524,#2989,#2990);
#2340=AXIS2_PLACEMENT_3D('',#3525,#2991,#2992);
#2341=AXIS2_PLACEMENT_3D('',#3526,#2993,#2994);
#2342=AXIS2_PLACEMENT_3D('',#3527,#2995,#2996);
#2343=AXIS2_PLACEMENT_3D('',#3528,#2997,#2998);
#2344=AXIS2_PLACEMENT_3D('',#3529,#2999,#3000);
#2345=AXIS2_PLACEMENT_3D('',#3530,#3001,#3002);
#2346=AXIS2_PLACEMENT_3D('',#3531,#3003,#3004);
#2347=AXIS2_PLACEMENT_3D('',#3532,#3005,#3006);
#2348=AXIS2_PLACEMENT_3D('',#3533,#3007,#3008);
#2349=AXIS2_PLACEMENT_3D('',#3534,#3009,#3010);
#2350=AXIS2_PLACEMENT_3D('',#3535,#3011,#3012);
#2351=AXIS2_PLACEMENT_3D('',#3536,#3013,#3014);
#2352=AXIS2_PLACEMENT_3D('',#3537,#3015,#3016);
#2353=AXIS2_PLACEMENT_3D('',#3538,#3017,#3018);
#2354=AXIS2_PLACEMENT_3D('',#3539,#3019,#3020);
#2355=AXIS2_PLACEMENT_3D('',#3540,#3021,#3022);
#2356=AXIS2_PLACEMENT_3D('',#3541,#3023,#3024);
#2357=AXIS2_PLACEMENT_3D('',#3542,#3025,#3026);
#2358=AXIS2_PLACEMENT_3D('',#3543,#3027,#3028);
#2359=DIRECTION('axis',(0.,0.,1.));
#2360=DIRECTION('refdir',(1.,0.,0.));
#2361=DIRECTION('axis',(0.,0.,1.));
#2362=DIRECTION('refdir',(1.,0.,0.));
#2363=DIRECTION('center_axis',(0.,0.,-1.));
#2364=DIRECTION('ref_axis',(1.,0.,0.));
#2365=DIRECTION('center_axis',(0.,0.,-1.));
#2366=DIRECTION('ref_axis',(1.,0.,0.));
#2367=DIRECTION('',(0.,0.,-1.));
#2368=DIRECTION('center_axis',(0.,0.,1.));
#2369=DIRECTION('ref_axis',(1.,0.,0.));
#2370=DIRECTION('center_axis',(0.,0.,-1.));
#2371=DIRECTION('ref_axis',(1.,0.,0.));
#2372=DIRECTION('center_axis',(0.,0.,-1.));
#2373=DIRECTION('ref_axis',(1.,0.,0.));
#2374=DIRECTION('',(0.,0.,-1.));
#2375=DIRECTION('center_axis',(0.,0.,1.));
#2376=DIRECTION('ref_axis',(1.,0.,0.));
#2377=DIRECTION('center_axis',(0.,0.,-1.));
#2378=DIRECTION('ref_axis',(1.,0.,0.));
#2379=DIRECTION('center_axis',(0.,0.,-1.));
#2380=DIRECTION('ref_axis',(1.,0.,0.));
#2381=DIRECTION('',(0.,0.,-1.));
#2382=DIRECTION('center_axis',(0.,0.,1.));
#2383=DIRECTION('ref_axis',(1.,0.,0.));
#2384=DIRECTION('center_axis',(0.,0.,-1.));
#2385=DIRECTION('ref_axis',(1.,0.,0.));
#2386=DIRECTION('center_axis',(0.,0.,-1.));
#2387=DIRECTION('ref_axis',(1.,0.,0.));
#2388=DIRECTION('',(0.,0.,-1.));
#2389=DIRECTION('center_axis',(0.,0.,1.));
#2390=DIRECTION('ref_axis',(1.,0.,0.));
#2391=DIRECTION('center_axis',(0.,0.,-1.));
#2392=DIRECTION('ref_axis',(1.,0.,0.));
#2393=DIRECTION('center_axis',(0.,0.,-1.));
#2394=DIRECTION('ref_axis',(1.,0.,0.));
#2395=DIRECTION('',(0.,0.,-1.));
#2396=DIRECTION('center_axis',(0.,0.,1.));
#2397=DIRECTION('ref_axis',(1.,0.,0.));
#2398=DIRECTION('center_axis',(0.,1.,0.));
#2399=DIRECTION('ref_axis',(-1.,0.,0.));
#2400=DIRECTION('',(1.,0.,0.));
#2401=DIRECTION('',(0.,0.,1.));
#2402=DIRECTION('',(1.,0.,0.));
#2403=DIRECTION('',(0.,0.,-1.));
#2404=DIRECTION('center_axis',(1.,0.,0.));
#2405=DIRECTION('ref_axis',(0.,1.,0.));
#2406=DIRECTION('',(0.,-1.,0.));
#2407=DIRECTION('',(0.,-1.,0.));
#2408=DIRECTION('',(0.,0.,-1.));
#2409=DIRECTION('center_axis',(0.,-1.,0.));
#2410=DIRECTION('ref_axis',(1.,0.,0.));
#2411=DIRECTION('',(-1.,0.,0.));
#2412=DIRECTION('',(-1.,0.,0.));
#2413=DIRECTION('',(0.,0.,1.));
#2414=DIRECTION('center_axis',(-1.,0.,0.));
#2415=DIRECTION('ref_axis',(0.,-1.,0.));
#2416=DIRECTION('',(0.,1.,0.));
#2417=DIRECTION('',(0.,1.,0.));
#2418=DIRECTION('center_axis',(0.,0.,1.));
#2419=DIRECTION('ref_axis',(1.,0.,0.));
#2420=DIRECTION('center_axis',(0.,0.,1.));
#2421=DIRECTION('ref_axis',(1.,0.,0.));
#2422=DIRECTION('axis',(0.,0.,1.));
#2423=DIRECTION('refdir',(1.,0.,0.));
#2424=DIRECTION('center_axis',(0.,0.,1.));
#2425=DIRECTION('ref_axis',(1.,0.,0.));
#2426=DIRECTION('center_axis',(0.,0.,-1.));
#2427=DIRECTION('ref_axis',(1.,0.,0.));
#2428=DIRECTION('',(0.,0.,-1.));
#2429=DIRECTION('center_axis',(0.,0.,-1.));
#2430=DIRECTION('ref_axis',(1.,0.,0.));
#2431=DIRECTION('center_axis',(0.,0.,1.));
#2432=DIRECTION('ref_axis',(1.,0.,0.));
#2433=DIRECTION('center_axis',(0.,0.,-1.));
#2434=DIRECTION('ref_axis',(1.,0.,0.));
#2435=DIRECTION('',(0.,0.,-1.));
#2436=DIRECTION('center_axis',(0.,0.,-1.));
#2437=DIRECTION('ref_axis',(1.,0.,0.));
#2438=DIRECTION('center_axis',(0.,0.,1.));
#2439=DIRECTION('ref_axis',(1.,0.,0.));
#2440=DIRECTION('center_axis',(0.,0.,1.));
#2441=DIRECTION('ref_axis',(1.,0.,0.));
#2442=DIRECTION('axis',(0.,0.,1.));
#2443=DIRECTION('refdir',(1.,0.,0.));
#2444=DIRECTION('center_axis',(0.,0.,-1.));
#2445=DIRECTION('ref_axis',(1.,0.,0.));
#2446=DIRECTION('center_axis',(0.,0.,-1.));
#2447=DIRECTION('ref_axis',(1.,0.,0.));
#2448=DIRECTION('',(0.,0.,-1.));
#2449=DIRECTION('center_axis',(0.,0.,1.));
#2450=DIRECTION('ref_axis',(1.,0.,0.));
#2451=DIRECTION('center_axis',(0.,1.,0.));
#2452=DIRECTION('ref_axis',(-1.,0.,0.));
#2453=DIRECTION('',(-1.,0.,0.));
#2454=DIRECTION('',(0.,0.,1.));
#2455=DIRECTION('',(-1.,0.,0.));
#2456=DIRECTION('',(0.,0.,1.));
#2457=DIRECTION('center_axis',(1.,0.,0.));
#2458=DIRECTION('ref_axis',(0.,1.,0.));
#2459=DIRECTION('',(0.,1.,0.));
#2460=DIRECTION('',(0.,1.,0.));
#2461=DIRECTION('',(0.,0.,1.));
#2462=DIRECTION('center_axis',(0.,-1.,0.));
#2463=DIRECTION('ref_axis',(1.,0.,0.));
#2464=DIRECTION('',(1.,0.,0.));
#2465=DIRECTION('',(1.,0.,0.));
#2466=DIRECTION('',(0.,0.,1.));
#2467=DIRECTION('center_axis',(-1.,0.,0.));
#2468=DIRECTION('ref_axis',(0.,-1.,0.));
#2469=DIRECTION('',(0.,-1.,0.));
#2470=DIRECTION('',(0.,-1.,0.));
#2471=DIRECTION('center_axis',(0.,0.,1.));
#2472=DIRECTION('ref_axis',(1.,0.,0.));
#2473=DIRECTION('center_axis',(0.,0.,1.));
#2474=DIRECTION('ref_axis',(1.,0.,0.));
#2475=DIRECTION('axis',(0.,0.,1.));
#2476=DIRECTION('refdir',(1.,0.,0.));
#2477=DIRECTION('center_axis',(0.,0.,-1.));
#2478=DIRECTION('ref_axis',(1.,0.,0.));
#2479=DIRECTION('center_axis',(0.,0.,-1.));
#2480=DIRECTION('ref_axis',(1.,0.,0.));
#2481=DIRECTION('',(0.,0.,-1.));
#2482=DIRECTION('center_axis',(0.,0.,1.));
#2483=DIRECTION('ref_axis',(1.,0.,0.));
#2484=DIRECTION('center_axis',(0.,0.,-1.));
#2485=DIRECTION('ref_axis',(1.,0.,0.));
#2486=DIRECTION('center_axis',(0.,0.,-1.));
#2487=DIRECTION('ref_axis',(1.,0.,0.));
#2488=DIRECTION('',(0.,0.,-1.));
#2489=DIRECTION('center_axis',(0.,0.,1.));
#2490=DIRECTION('ref_axis',(1.,0.,0.));
#2491=DIRECTION('center_axis',(0.,1.,0.));
#2492=DIRECTION('ref_axis',(-1.,0.,0.));
#2493=DIRECTION('',(-1.,0.,0.));
#2494=DIRECTION('',(0.,0.,1.));
#2495=DIRECTION('',(-1.,0.,0.));
#2496=DIRECTION('',(0.,0.,1.));
#2497=DIRECTION('center_axis',(0.,0.,1.));
#2498=DIRECTION('ref_axis',(0.,-1.,0.));
#2499=DIRECTION('center_axis',(0.,0.,1.));
#2500=DIRECTION('ref_axis',(0.,-1.,0.));
#2501=DIRECTION('center_axis',(0.,0.,1.));
#2502=DIRECTION('ref_axis',(0.,-1.,0.));
#2503=DIRECTION('',(0.,0.,1.));
#2504=DIRECTION('center_axis',(0.,-1.,0.));
#2505=DIRECTION('ref_axis',(1.,0.,0.));
#2506=DIRECTION('',(1.,0.,0.));
#2507=DIRECTION('',(1.,0.,0.));
#2508=DIRECTION('',(0.,0.,1.));
#2509=DIRECTION('center_axis',(0.,0.,1.));
#2510=DIRECTION('ref_axis',(0.,1.,0.));
#2511=DIRECTION('center_axis',(0.,0.,1.));
#2512=DIRECTION('ref_axis',(0.,1.,0.));
#2513=DIRECTION('center_axis',(0.,0.,1.));
#2514=DIRECTION('ref_axis',(0.,1.,0.));
#2515=DIRECTION('center_axis',(0.,0.,1.));
#2516=DIRECTION('ref_axis',(1.,0.,0.));
#2517=DIRECTION('center_axis',(0.,0.,1.));
#2518=DIRECTION('ref_axis',(1.,0.,0.));
#2519=DIRECTION('axis',(0.,0.,1.));
#2520=DIRECTION('refdir',(1.,0.,0.));
#2521=DIRECTION('center_axis',(0.,0.,1.));
#2522=DIRECTION('ref_axis',(1.,0.,0.));
#2523=DIRECTION('center_axis',(0.,0.,1.));
#2524=DIRECTION('ref_axis',(1.,0.,0.));
#2525=DIRECTION('',(0.,0.,-1.));
#2526=DIRECTION('center_axis',(0.,0.,1.));
#2527=DIRECTION('ref_axis',(1.,0.,0.));
#2528=DIRECTION('center_axis',(0.,0.,1.));
#2529=DIRECTION('ref_axis',(1.,0.,0.));
#2530=DIRECTION('center_axis',(0.,0.,1.));
#2531=DIRECTION('ref_axis',(1.,0.,0.));
#2532=DIRECTION('axis',(0.,0.,1.));
#2533=DIRECTION('refdir',(1.,0.,0.));
#2534=DIRECTION('center_axis',(0.,0.,-1.));
#2535=DIRECTION('ref_axis',(1.,0.,0.));
#2536=DIRECTION('center_axis',(0.,0.,-1.));
#2537=DIRECTION('ref_axis',(1.,0.,0.));
#2538=DIRECTION('',(0.,0.,-1.));
#2539=DIRECTION('center_axis',(0.,0.,1.));
#2540=DIRECTION('ref_axis',(1.,0.,0.));
#2541=DIRECTION('center_axis',(0.,0.,-1.));
#2542=DIRECTION('ref_axis',(1.,0.,0.));
#2543=DIRECTION('center_axis',(0.,0.,-1.));
#2544=DIRECTION('ref_axis',(1.,0.,0.));
#2545=DIRECTION('',(0.,0.,-1.));
#2546=DIRECTION('center_axis',(0.,0.,1.));
#2547=DIRECTION('ref_axis',(1.,0.,0.));
#2548=DIRECTION('center_axis',(0.,1.,0.));
#2549=DIRECTION('ref_axis',(-1.,0.,0.));
#2550=DIRECTION('',(-1.,0.,0.));
#2551=DIRECTION('',(0.,0.,1.));
#2552=DIRECTION('',(-1.,0.,0.));
#2553=DIRECTION('',(0.,0.,1.));
#2554=DIRECTION('center_axis',(0.,0.,1.));
#2555=DIRECTION('ref_axis',(0.,-1.,0.));
#2556=DIRECTION('center_axis',(0.,0.,1.));
#2557=DIRECTION('ref_axis',(0.,-1.,0.));
#2558=DIRECTION('center_axis',(0.,0.,1.));
#2559=DIRECTION('ref_axis',(0.,-1.,0.));
#2560=DIRECTION('',(0.,0.,1.));
#2561=DIRECTION('center_axis',(0.,-1.,0.));
#2562=DIRECTION('ref_axis',(1.,0.,0.));
#2563=DIRECTION('',(1.,0.,0.));
#2564=DIRECTION('',(1.,0.,0.));
#2565=DIRECTION('',(0.,0.,1.));
#2566=DIRECTION('center_axis',(0.,0.,1.));
#2567=DIRECTION('ref_axis',(0.,1.,0.));
#2568=DIRECTION('center_axis',(0.,0.,1.));
#2569=DIRECTION('ref_axis',(0.,1.,0.));
#2570=DIRECTION('center_axis',(0.,0.,1.));
#2571=DIRECTION('ref_axis',(0.,1.,0.));
#2572=DIRECTION('center_axis',(0.,0.,1.));
#2573=DIRECTION('ref_axis',(1.,0.,0.));
#2574=DIRECTION('center_axis',(0.,0.,1.));
#2575=DIRECTION('ref_axis',(1.,0.,0.));
#2576=DIRECTION('axis',(0.,0.,1.));
#2577=DIRECTION('refdir',(1.,0.,0.));
#2578=DIRECTION('center_axis',(0.,0.,-1.));
#2579=DIRECTION('ref_axis',(1.,0.,0.));
#2580=DIRECTION('center_axis',(0.,0.,-1.));
#2581=DIRECTION('ref_axis',(1.,0.,0.));
#2582=DIRECTION('',(0.,0.,-1.));
#2583=DIRECTION('center_axis',(0.,0.,1.));
#2584=DIRECTION('ref_axis',(1.,0.,0.));
#2585=DIRECTION('center_axis',(0.,0.,-1.));
#2586=DIRECTION('ref_axis',(1.,0.,0.));
#2587=DIRECTION('center_axis',(0.,0.,-1.));
#2588=DIRECTION('ref_axis',(1.,0.,0.));
#2589=DIRECTION('',(0.,0.,-1.));
#2590=DIRECTION('center_axis',(0.,0.,1.));
#2591=DIRECTION('ref_axis',(1.,0.,0.));
#2592=DIRECTION('center_axis',(0.,1.,0.));
#2593=DIRECTION('ref_axis',(-1.,0.,0.));
#2594=DIRECTION('',(-1.,0.,0.));
#2595=DIRECTION('',(0.,0.,1.));
#2596=DIRECTION('',(-1.,0.,0.));
#2597=DIRECTION('',(0.,0.,1.));
#2598=DIRECTION('center_axis',(0.,0.,1.));
#2599=DIRECTION('ref_axis',(0.,-1.,0.));
#2600=DIRECTION('center_axis',(0.,0.,1.));
#2601=DIRECTION('ref_axis',(0.,-1.,0.));
#2602=DIRECTION('center_axis',(0.,0.,1.));
#2603=DIRECTION('ref_axis',(0.,-1.,0.));
#2604=DIRECTION('',(0.,0.,1.));
#2605=DIRECTION('center_axis',(0.,-1.,0.));
#2606=DIRECTION('ref_axis',(1.,0.,0.));
#2607=DIRECTION('',(1.,0.,0.));
#2608=DIRECTION('',(1.,0.,0.));
#2609=DIRECTION('',(0.,0.,1.));
#2610=DIRECTION('center_axis',(0.,0.,1.));
#2611=DIRECTION('ref_axis',(0.,1.,0.));
#2612=DIRECTION('center_axis',(0.,0.,1.));
#2613=DIRECTION('ref_axis',(0.,1.,0.));
#2614=DIRECTION('center_axis',(0.,0.,1.));
#2615=DIRECTION('ref_axis',(0.,1.,0.));
#2616=DIRECTION('center_axis',(0.,0.,1.));
#2617=DIRECTION('ref_axis',(1.,0.,0.));
#2618=DIRECTION('center_axis',(0.,0.,1.));
#2619=DIRECTION('ref_axis',(1.,0.,0.));
#2620=DIRECTION('axis',(0.,0.,1.));
#2621=DIRECTION('refdir',(1.,0.,0.));
#2622=DIRECTION('center_axis',(0.,0.,1.));
#2623=DIRECTION('ref_axis',(1.,0.,0.));
#2624=DIRECTION('center_axis',(0.,0.,1.));
#2625=DIRECTION('ref_axis',(1.,0.,0.));
#2626=DIRECTION('',(0.,0.,1.));
#2627=DIRECTION('center_axis',(0.,0.,1.));
#2628=DIRECTION('ref_axis',(1.,0.,0.));
#2629=DIRECTION('center_axis',(0.,0.,-1.));
#2630=DIRECTION('ref_axis',(-1.,0.,0.));
#2631=DIRECTION('center_axis',(0.,0.,-1.));
#2632=DIRECTION('ref_axis',(1.,0.,0.));
#2633=DIRECTION('center_axis',(0.,0.,1.));
#2634=DIRECTION('ref_axis',(1.,0.,0.));
#2635=DIRECTION('center_axis',(0.,0.,1.));
#2636=DIRECTION('ref_axis',(1.,0.,0.));
#2637=DIRECTION('center_axis',(0.,0.,1.));
#2638=DIRECTION('ref_axis',(1.,0.,0.));
#2639=DIRECTION('center_axis',(0.,0.,1.));
#2640=DIRECTION('ref_axis',(1.,0.,0.));
#2641=DIRECTION('',(0.,0.,-1.));
#2642=DIRECTION('center_axis',(0.,0.,1.));
#2643=DIRECTION('ref_axis',(1.,0.,0.));
#2644=DIRECTION('center_axis',(0.,0.,1.));
#2645=DIRECTION('ref_axis',(1.,0.,0.));
#2646=DIRECTION('center_axis',(0.,0.,1.));
#2647=DIRECTION('ref_axis',(1.,0.,0.));
#2648=DIRECTION('center_axis',(0.,0.,1.));
#2649=DIRECTION('ref_axis',(1.,0.,0.));
#2650=DIRECTION('',(0.,0.,-1.));
#2651=DIRECTION('center_axis',(0.,0.,1.));
#2652=DIRECTION('ref_axis',(1.,0.,0.));
#2653=DIRECTION('center_axis',(0.,0.,1.));
#2654=DIRECTION('ref_axis',(1.,0.,0.));
#2655=DIRECTION('center_axis',(0.,0.,1.));
#2656=DIRECTION('ref_axis',(1.,0.,0.));
#2657=DIRECTION('',(0.,0.,-1.));
#2658=DIRECTION('center_axis',(0.,0.,1.));
#2659=DIRECTION('ref_axis',(1.,0.,0.));
#2660=DIRECTION('axis',(0.,0.,1.));
#2661=DIRECTION('refdir',(1.,0.,0.));
#2662=DIRECTION('center_axis',(0.,0.,1.));
#2663=DIRECTION('ref_axis',(1.,0.,0.));
#2664=DIRECTION('center_axis',(0.,0.,1.));
#2665=DIRECTION('ref_axis',(1.,0.,0.));
#2666=DIRECTION('',(0.,0.,1.));
#2667=DIRECTION('center_axis',(0.,0.,1.));
#2668=DIRECTION('ref_axis',(1.,0.,0.));
#2669=DIRECTION('center_axis',(0.,0.,-1.));
#2670=DIRECTION('ref_axis',(-1.,0.,0.));
#2671=DIRECTION('center_axis',(0.,0.,-1.));
#2672=DIRECTION('ref_axis',(1.,0.,0.));
#2673=DIRECTION('center_axis',(0.,0.,1.));
#2674=DIRECTION('ref_axis',(1.,0.,0.));
#2675=DIRECTION('center_axis',(0.,0.,1.));
#2676=DIRECTION('ref_axis',(1.,0.,0.));
#2677=DIRECTION('center_axis',(0.,0.,1.));
#2678=DIRECTION('ref_axis',(1.,0.,0.));
#2679=DIRECTION('center_axis',(0.,0.,1.));
#2680=DIRECTION('ref_axis',(1.,0.,0.));
#2681=DIRECTION('',(0.,0.,-1.));
#2682=DIRECTION('center_axis',(0.,0.,1.));
#2683=DIRECTION('ref_axis',(1.,0.,0.));
#2684=DIRECTION('center_axis',(0.,0.,1.));
#2685=DIRECTION('ref_axis',(1.,0.,0.));
#2686=DIRECTION('center_axis',(0.,0.,1.));
#2687=DIRECTION('ref_axis',(1.,0.,0.));
#2688=DIRECTION('center_axis',(0.,0.,1.));
#2689=DIRECTION('ref_axis',(1.,0.,0.));
#2690=DIRECTION('',(0.,0.,-1.));
#2691=DIRECTION('center_axis',(0.,0.,1.));
#2692=DIRECTION('ref_axis',(1.,0.,0.));
#2693=DIRECTION('center_axis',(0.,0.,1.));
#2694=DIRECTION('ref_axis',(1.,0.,0.));
#2695=DIRECTION('center_axis',(0.,0.,1.));
#2696=DIRECTION('ref_axis',(1.,0.,0.));
#2697=DIRECTION('',(0.,0.,-1.));
#2698=DIRECTION('center_axis',(0.,0.,1.));
#2699=DIRECTION('ref_axis',(1.,0.,0.));
#2700=DIRECTION('axis',(0.,0.,1.));
#2701=DIRECTION('refdir',(1.,0.,0.));
#2702=DIRECTION('center_axis',(0.,0.,1.));
#2703=DIRECTION('ref_axis',(1.,0.,0.));
#2704=DIRECTION('center_axis',(0.,0.,-1.));
#2705=DIRECTION('ref_axis',(1.,0.,0.));
#2706=DIRECTION('',(0.,0.,-1.));
#2707=DIRECTION('center_axis',(0.,0.,-1.));
#2708=DIRECTION('ref_axis',(1.,0.,0.));
#2709=DIRECTION('center_axis',(0.,0.,1.));
#2710=DIRECTION('ref_axis',(1.,0.,0.));
#2711=DIRECTION('center_axis',(0.,0.,1.));
#2712=DIRECTION('ref_axis',(1.,0.,0.));
#2713=DIRECTION('',(0.,0.,-1.));
#2714=DIRECTION('center_axis',(0.,0.,1.));
#2715=DIRECTION('ref_axis',(1.,0.,0.));
#2716=DIRECTION('center_axis',(0.,0.,1.));
#2717=DIRECTION('ref_axis',(1.,0.,0.));
#2718=DIRECTION('center_axis',(0.,0.,1.));
#2719=DIRECTION('ref_axis',(1.,0.,0.));
#2720=DIRECTION('axis',(0.,0.,1.));
#2721=DIRECTION('refdir',(1.,0.,0.));
#2722=DIRECTION('center_axis',(0.,0.,1.));
#2723=DIRECTION('ref_axis',(1.,0.,0.));
#2724=DIRECTION('center_axis',(0.,0.,1.));
#2725=DIRECTION('ref_axis',(1.,0.,0.));
#2726=DIRECTION('',(0.,0.,1.));
#2727=DIRECTION('center_axis',(0.,0.,1.));
#2728=DIRECTION('ref_axis',(1.,0.,0.));
#2729=DIRECTION('center_axis',(0.,0.,-1.));
#2730=DIRECTION('ref_axis',(-1.,0.,0.));
#2731=DIRECTION('center_axis',(0.,0.,-1.));
#2732=DIRECTION('ref_axis',(1.,0.,0.));
#2733=DIRECTION('center_axis',(0.,0.,1.));
#2734=DIRECTION('ref_axis',(1.,0.,0.));
#2735=DIRECTION('center_axis',(0.,0.,1.));
#2736=DIRECTION('ref_axis',(1.,0.,0.));
#2737=DIRECTION('center_axis',(0.,0.,1.));
#2738=DIRECTION('ref_axis',(1.,0.,0.));
#2739=DIRECTION('center_axis',(0.,0.,1.));
#2740=DIRECTION('ref_axis',(1.,0.,0.));
#2741=DIRECTION('',(0.,0.,-1.));
#2742=DIRECTION('center_axis',(0.,0.,1.));
#2743=DIRECTION('ref_axis',(1.,0.,0.));
#2744=DIRECTION('center_axis',(0.,0.,1.));
#2745=DIRECTION('ref_axis',(1.,0.,0.));
#2746=DIRECTION('center_axis',(0.,0.,1.));
#2747=DIRECTION('ref_axis',(1.,0.,0.));
#2748=DIRECTION('center_axis',(0.,0.,1.));
#2749=DIRECTION('ref_axis',(1.,0.,0.));
#2750=DIRECTION('',(0.,0.,-1.));
#2751=DIRECTION('center_axis',(0.,0.,1.));
#2752=DIRECTION('ref_axis',(1.,0.,0.));
#2753=DIRECTION('center_axis',(0.,0.,1.));
#2754=DIRECTION('ref_axis',(1.,0.,0.));
#2755=DIRECTION('center_axis',(0.,0.,-1.));
#2756=DIRECTION('ref_axis',(1.,0.,0.));
#2757=DIRECTION('center_axis',(0.,0.,1.));
#2758=DIRECTION('ref_axis',(1.,0.,0.));
#2759=DIRECTION('center_axis',(0.,0.,-1.));
#2760=DIRECTION('ref_axis',(1.,0.,0.));
#2761=DIRECTION('',(0.,0.,-1.));
#2762=DIRECTION('center_axis',(0.,0.,1.));
#2763=DIRECTION('ref_axis',(1.,0.,0.));
#2764=DIRECTION('',(0.,0.,-1.));
#2765=DIRECTION('center_axis',(0.,0.,1.));
#2766=DIRECTION('ref_axis',(1.,0.,0.));
#2767=DIRECTION('axis',(0.,0.,1.));
#2768=DIRECTION('refdir',(1.,0.,0.));
#2769=DIRECTION('center_axis',(0.,0.,1.));
#2770=DIRECTION('ref_axis',(1.,0.,0.));
#2771=DIRECTION('center_axis',(0.,0.,-1.));
#2772=DIRECTION('ref_axis',(1.,0.,0.));
#2773=DIRECTION('',(0.,0.,-1.));
#2774=DIRECTION('center_axis',(0.,0.,-1.));
#2775=DIRECTION('ref_axis',(1.,0.,0.));
#2776=DIRECTION('center_axis',(0.,0.,1.));
#2777=DIRECTION('ref_axis',(1.,0.,0.));
#2778=DIRECTION('center_axis',(0.,0.,1.));
#2779=DIRECTION('ref_axis',(1.,0.,0.));
#2780=DIRECTION('',(0.,0.,-1.));
#2781=DIRECTION('center_axis',(0.,0.,1.));
#2782=DIRECTION('ref_axis',(1.,0.,0.));
#2783=DIRECTION('center_axis',(0.,0.,1.));
#2784=DIRECTION('ref_axis',(1.,0.,0.));
#2785=DIRECTION('center_axis',(0.,0.,1.));
#2786=DIRECTION('ref_axis',(1.,0.,0.));
#2787=DIRECTION('axis',(0.,0.,1.));
#2788=DIRECTION('refdir',(1.,0.,0.));
#2789=DIRECTION('center_axis',(0.,0.,1.));
#2790=DIRECTION('ref_axis',(1.,0.,0.));
#2791=DIRECTION('center_axis',(0.,0.,1.));
#2792=DIRECTION('ref_axis',(1.,0.,0.));
#2793=DIRECTION('',(0.,0.,-1.));
#2794=DIRECTION('center_axis',(0.,0.,1.));
#2795=DIRECTION('ref_axis',(1.,0.,0.));
#2796=DIRECTION('center_axis',(0.,0.,1.));
#2797=DIRECTION('ref_axis',(1.,0.,0.));
#2798=DIRECTION('center_axis',(0.,0.,1.));
#2799=DIRECTION('ref_axis',(1.,0.,0.));
#2800=DIRECTION('',(0.447213595499958,5.47678698264203E-17,-0.894427190999916));
#2801=DIRECTION('axis',(0.,0.,1.));
#2802=DIRECTION('refdir',(1.,0.,0.));
#2803=DIRECTION('center_axis',(0.,0.,1.));
#2804=DIRECTION('ref_axis',(1.,0.,0.));
#2805=DIRECTION('center_axis',(0.,0.,1.));
#2806=DIRECTION('ref_axis',(1.,0.,0.));
#2807=DIRECTION('',(0.,0.,1.));
#2808=DIRECTION('center_axis',(0.,0.,1.));
#2809=DIRECTION('ref_axis',(1.,0.,0.));
#2810=DIRECTION('center_axis',(0.,0.,-1.));
#2811=DIRECTION('ref_axis',(-1.,0.,0.));
#2812=DIRECTION('center_axis',(0.,0.,-1.));
#2813=DIRECTION('ref_axis',(1.,0.,0.));
#2814=DIRECTION('center_axis',(0.,0.,1.));
#2815=DIRECTION('ref_axis',(1.,0.,0.));
#2816=DIRECTION('center_axis',(0.,0.,1.));
#2817=DIRECTION('ref_axis',(1.,0.,0.));
#2818=DIRECTION('center_axis',(0.,0.,1.));
#2819=DIRECTION('ref_axis',(1.,0.,0.));
#2820=DIRECTION('center_axis',(0.,0.,1.));
#2821=DIRECTION('ref_axis',(1.,0.,0.));
#2822=DIRECTION('',(0.,0.,-1.));
#2823=DIRECTION('center_axis',(0.,0.,1.));
#2824=DIRECTION('ref_axis',(1.,0.,0.));
#2825=DIRECTION('center_axis',(0.,0.,1.));
#2826=DIRECTION('ref_axis',(1.,0.,0.));
#2827=DIRECTION('center_axis',(0.,0.,1.));
#2828=DIRECTION('ref_axis',(1.,0.,0.));
#2829=DIRECTION('center_axis',(0.,0.,1.));
#2830=DIRECTION('ref_axis',(1.,0.,0.));
#2831=DIRECTION('',(0.,0.,-1.));
#2832=DIRECTION('center_axis',(0.,0.,1.));
#2833=DIRECTION('ref_axis',(1.,0.,0.));
#2834=DIRECTION('center_axis',(0.,0.,1.));
#2835=DIRECTION('ref_axis',(1.,0.,0.));
#2836=DIRECTION('center_axis',(0.,0.,1.));
#2837=DIRECTION('ref_axis',(1.,0.,0.));
#2838=DIRECTION('',(0.,0.,-1.));
#2839=DIRECTION('center_axis',(0.,0.,1.));
#2840=DIRECTION('ref_axis',(1.,0.,0.));
#2841=DIRECTION('axis',(0.,0.,1.));
#2842=DIRECTION('refdir',(1.,0.,0.));
#2843=DIRECTION('center_axis',(0.,0.,1.));
#2844=DIRECTION('ref_axis',(1.,0.,0.));
#2845=DIRECTION('center_axis',(0.,0.,-1.));
#2846=DIRECTION('ref_axis',(1.,0.,0.));
#2847=DIRECTION('',(0.,0.,-1.));
#2848=DIRECTION('center_axis',(0.,0.,-1.));
#2849=DIRECTION('ref_axis',(1.,0.,0.));
#2850=DIRECTION('center_axis',(0.,0.,1.));
#2851=DIRECTION('ref_axis',(1.,0.,0.));
#2852=DIRECTION('center_axis',(0.,0.,1.));
#2853=DIRECTION('ref_axis',(1.,0.,0.));
#2854=DIRECTION('',(0.,0.,-1.));
#2855=DIRECTION('center_axis',(0.,0.,1.));
#2856=DIRECTION('ref_axis',(1.,0.,0.));
#2857=DIRECTION('center_axis',(0.,0.,1.));
#2858=DIRECTION('ref_axis',(1.,0.,0.));
#2859=DIRECTION('center_axis',(0.,0.,1.));
#2860=DIRECTION('ref_axis',(1.,0.,0.));
#2861=DIRECTION('axis',(0.,0.,1.));
#2862=DIRECTION('refdir',(1.,0.,0.));
#2863=DIRECTION('center_axis',(0.,0.,1.));
#2864=DIRECTION('ref_axis',(1.,0.,0.));
#2865=DIRECTION('center_axis',(0.,0.,-1.));
#2866=DIRECTION('ref_axis',(1.,0.,0.));
#2867=DIRECTION('',(0.,0.,-1.));
#2868=DIRECTION('center_axis',(0.,0.,-1.));
#2869=DIRECTION('ref_axis',(1.,0.,0.));
#2870=DIRECTION('center_axis',(0.,0.,1.));
#2871=DIRECTION('ref_axis',(1.,0.,0.));
#2872=DIRECTION('center_axis',(0.,0.,1.));
#2873=DIRECTION('ref_axis',(1.,0.,0.));
#2874=DIRECTION('',(0.,0.,-1.));
#2875=DIRECTION('center_axis',(0.,0.,1.));
#2876=DIRECTION('ref_axis',(1.,0.,0.));
#2877=DIRECTION('center_axis',(0.,0.,1.));
#2878=DIRECTION('ref_axis',(1.,0.,0.));
#2879=DIRECTION('center_axis',(0.,0.,1.));
#2880=DIRECTION('ref_axis',(1.,0.,0.));
#2881=DIRECTION('axis',(0.,0.,1.));
#2882=DIRECTION('refdir',(1.,0.,0.));
#2883=DIRECTION('center_axis',(-1.,0.,0.));
#2884=DIRECTION('ref_axis',(0.,1.,0.));
#2885=DIRECTION('',(0.,0.,1.));
#2886=DIRECTION('',(0.,-1.,0.));
#2887=DIRECTION('',(0.,0.,-1.));
#2888=DIRECTION('',(0.,1.,0.));
#2889=DIRECTION('center_axis',(1.,0.,0.));
#2890=DIRECTION('ref_axis',(0.,-1.,0.));
#2891=DIRECTION('',(0.,0.,-1.));
#2892=DIRECTION('',(0.,-1.,0.));
#2893=DIRECTION('',(0.,0.,1.));
#2894=DIRECTION('',(0.,1.,0.));
#2895=DIRECTION('center_axis',(0.,0.,1.));
#2896=DIRECTION('ref_axis',(1.,0.,0.));
#2897=DIRECTION('center_axis',(0.,0.,1.));
#2898=DIRECTION('ref_axis',(1.,0.,0.));
#2899=DIRECTION('center_axis',(0.,0.,-1.));
#2900=DIRECTION('ref_axis',(1.,0.,0.));
#2901=DIRECTION('center_axis',(0.,0.,1.));
#2902=DIRECTION('ref_axis',(6.12323399573677E-17,-1.,0.));
#2903=DIRECTION('center_axis',(0.,0.,-1.));
#2904=DIRECTION('ref_axis',(1.,0.,0.));
#2905=DIRECTION('center_axis',(0.,0.,1.));
#2906=DIRECTION('ref_axis',(6.12323399573677E-17,-1.,0.));
#2907=DIRECTION('center_axis',(0.,0.,1.));
#2908=DIRECTION('ref_axis',(1.,0.,0.));
#2909=DIRECTION('center_axis',(0.,0.,1.));
#2910=DIRECTION('ref_axis',(1.,0.,0.));
#2911=DIRECTION('',(0.,0.,1.));
#2912=DIRECTION('',(1.,0.,0.));
#2913=DIRECTION('',(0.,0.,1.));
#2914=DIRECTION('',(1.,0.,0.));
#2915=DIRECTION('',(0.,0.,1.));
#2916=DIRECTION('',(1.,0.,0.));
#2917=DIRECTION('',(0.,0.,1.));
#2918=DIRECTION('',(1.,0.,0.));
#2919=DIRECTION('',(3.48332022315797E-17,-6.12323399573948E-17,1.00000000000003));
#2920=DIRECTION('',(0.890799515546355,0.454396548294957,-3.20563575215545E-18));
#2921=DIRECTION('',(1.23171528715031E-16,-9.50099299702446E-17,1.00000000000002));
#2922=DIRECTION('',(-0.437253366852414,-0.89933836411899,-3.15889093634943E-17));
#2923=DIRECTION('',(6.12323399569043E-17,-3.44926943328803E-17,1.00000000000003));
#2924=DIRECTION('',(0.963898423234107,-0.266270219301362,-6.82061332197052E-17));
#2925=DIRECTION('',(3.48332022315797E-17,-6.12323399573948E-17,1.00000000000003));
#2926=DIRECTION('',(0.990535610992275,-0.137255977487871,-4.29080319299963E-17));
#2927=DIRECTION('',(0.,0.,1.));
#2928=DIRECTION('',(1.,0.,0.));
#2929=DIRECTION('',(-2.65212689772506E-17,-6.12323399572885E-17,1.00000000000002));
#2930=DIRECTION('',(0.737647979888556,-0.675185498782612,-2.17798275105393E-17));
#2931=DIRECTION('',(6.16553758263104E-17,-3.40627245626594E-17,1.00000000000002));
#2932=DIRECTION('',(-0.182000807422743,0.983298381010293,4.47151500976043E-17));
#2933=DIRECTION('',(9.56752053399733E-17,3.25041224561462E-18,1.00000000000002));
#2934=DIRECTION('',(0.18200080742274,-0.983298381010293,-1.42168395234851E-17));
#2935=DIRECTION('',(3.40178364942164E-17,6.40547525102609E-17,1.00000000000002));
#2936=DIRECTION('',(0.437253366852411,0.899338364118993,-7.24813098767539E-17));
#2937=DIRECTION('',(0.,0.,1.));
#2938=DIRECTION('',(1.,0.,0.));
#2939=DIRECTION('',(0.,-1.22464679914735E-16,-1.));
#2940=DIRECTION('',(1.,0.,0.));
#2941=DIRECTION('',(0.,0.,1.));
#2942=DIRECTION('',(1.,0.,0.));
#2943=DIRECTION('',(3.48332022315797E-17,-6.12323399573948E-17,1.00000000000003));
#2944=DIRECTION('',(0.990535610992275,-0.137255977487871,-4.29080319299963E-17));
#2945=DIRECTION('',(9.56752053399733E-17,3.25041224561462E-18,1.00000000000002));
#2946=DIRECTION('',(0.992607114562357,-0.121371809413001,-9.4573381092083E-17));
#2947=DIRECTION('',(3.48332022315797E-17,-6.12323399573948E-17,1.00000000000003));
#2948=DIRECTION('',(0.990535610992275,-0.137255977487871,-4.29080319299963E-17));
#2949=DIRECTION('',(0.,0.,1.));
#2950=DIRECTION('',(1.,0.,0.));
#2951=DIRECTION('',(3.48332022315797E-17,-6.12323399573948E-17,1.00000000000003));
#2952=DIRECTION('',(0.990535610992275,-0.137255977487871,-4.29080319299963E-17));
#2953=DIRECTION('',(-2.65212689772506E-17,-6.12323399572885E-17,1.00000000000002));
#2954=DIRECTION('',(0.991322892818808,-0.131449314084715,1.82421919965649E-17));
#2955=DIRECTION('',(-2.65212689772506E-17,-6.12323399572885E-17,1.00000000000002));
#2956=DIRECTION('',(0.991322892818808,-0.131449314084715,1.82421919965649E-17));
#2957=DIRECTION('',(1.23171528715031E-16,-9.50099299702446E-17,1.00000000000002));
#2958=DIRECTION('',(0.989090130927016,-0.147311618356366,-1.35823810007071E-16));
#2959=DIRECTION('',(1.23171528715031E-16,-9.50099299702446E-17,1.00000000000002));
#2960=DIRECTION('',(0.989090130927016,-0.147311618356366,-1.35823810007071E-16));
#2961=DIRECTION('',(6.16553758263104E-17,-3.40627245626594E-17,1.00000000000002));
#2962=DIRECTION('',(0.992607114562357,-0.121371809412998,-6.53338192099174E-17));
#2963=DIRECTION('',(6.16553758263104E-17,-3.40627245626594E-17,1.00000000000002));
#2964=DIRECTION('',(0.992607114562357,-0.121371809412998,-6.53338192099174E-17));
#2965=DIRECTION('',(9.56752053399733E-17,3.25041224561462E-18,1.00000000000002));
#2966=DIRECTION('',(0.992607114562357,-0.121371809413001,-9.4573381092083E-17));
#2967=DIRECTION('',(9.56752053399733E-17,3.25041224561462E-18,1.00000000000002));
#2968=DIRECTION('',(0.992607114562357,-0.121371809413001,-9.4573381092083E-17));
#2969=DIRECTION('',(3.40178364942164E-17,6.40547525102609E-17,1.00000000000002));
#2970=DIRECTION('',(0.989090130927018,-0.147311618356362,-2.42106970962161E-17));
#2971=DIRECTION('',(3.40178364942164E-17,6.40547525102609E-17,1.00000000000002));
#2972=DIRECTION('',(0.989090130927018,-0.147311618356362,-2.42106970962161E-17));
#2973=DIRECTION('',(6.12323399569043E-17,-3.44926943328803E-17,1.00000000000003));
#2974=DIRECTION('',(0.963898423234107,-0.266270219301362,-6.82061332197052E-17));
#2975=DIRECTION('',(6.12323399569043E-17,-3.44926943328803E-17,1.00000000000003));
#2976=DIRECTION('',(0.963898423234107,-0.266270219301362,-6.82061332197052E-17));
#2977=DIRECTION('',(0.,0.,1.));
#2978=DIRECTION('',(1.,0.,0.));
#2979=DIRECTION('',(9.56752053399733E-17,3.25041224561462E-18,1.00000000000002));
#2980=DIRECTION('',(0.992607114562357,-0.121371809413001,-9.4573381092083E-17));
#2981=DIRECTION('',(0.,0.,1.));
#2982=DIRECTION('',(1.,0.,0.));
#2983=DIRECTION('',(0.,0.,1.));
#2984=DIRECTION('',(1.,0.,0.));
#2985=DIRECTION('',(3.48332022315797E-17,-6.12323399573948E-17,1.00000000000003));
#2986=DIRECTION('',(0.990535610992275,-0.137255977487871,-4.29080319299963E-17));
#2987=DIRECTION('',(3.48332022315797E-17,-6.12323399573948E-17,1.00000000000003));
#2988=DIRECTION('',(0.990535610992275,-0.137255977487871,-4.29080319299963E-17));
#2989=DIRECTION('',(3.48332022315797E-17,-6.12323399573948E-17,1.00000000000003));
#2990=DIRECTION('',(0.990535610992275,-0.137255977487871,-4.29080319299963E-17));
#2991=DIRECTION('',(3.48332022315797E-17,-6.12323399573948E-17,1.00000000000003));
#2992=DIRECTION('',(0.990535610992275,-0.137255977487871,-4.29080319299963E-17));
#2993=DIRECTION('',(-2.65212689772506E-17,-6.12323399572885E-17,1.00000000000002));
#2994=DIRECTION('',(0.991322892818808,-0.131449314084715,1.82421919965649E-17));
#2995=DIRECTION('',(-2.65212689772506E-17,-6.12323399572885E-17,1.00000000000002));
#2996=DIRECTION('',(0.991322892818808,-0.131449314084715,1.82421919965649E-17));
#2997=DIRECTION('',(-2.65212689772506E-17,-6.12323399572885E-17,1.00000000000002));
#2998=DIRECTION('',(0.991322892818808,-0.131449314084715,1.82421919965649E-17));
#2999=DIRECTION('',(-2.65212689772506E-17,-6.12323399572885E-17,1.00000000000002));
#3000=DIRECTION('',(0.991322892818808,-0.131449314084715,1.82421919965649E-17));
#3001=DIRECTION('',(-2.65212689772506E-17,-6.12323399572885E-17,1.00000000000002));
#3002=DIRECTION('',(0.991322892818808,-0.131449314084715,1.82421919965649E-17));
#3003=DIRECTION('',(-2.65212689772506E-17,-6.12323399572885E-17,1.00000000000002));
#3004=DIRECTION('',(0.991322892818808,-0.131449314084715,1.82421919965649E-17));
#3005=DIRECTION('',(6.12323399569043E-17,-3.44926943328803E-17,1.00000000000003));
#3006=DIRECTION('',(0.963898423234107,-0.266270219301362,-6.82061332197052E-17));
#3007=DIRECTION('',(6.12323399569043E-17,-3.44926943328803E-17,1.00000000000003));
#3008=DIRECTION('',(0.963898423234107,-0.266270219301362,-6.82061332197052E-17));
#3009=DIRECTION('',(6.12323399569043E-17,-3.44926943328803E-17,1.00000000000003));
#3010=DIRECTION('',(0.963898423234107,-0.266270219301362,-6.82061332197052E-17));
#3011=DIRECTION('',(6.12323399569043E-17,-3.44926943328803E-17,1.00000000000003));
#3012=DIRECTION('',(0.963898423234107,-0.266270219301362,-6.82061332197052E-17));
#3013=DIRECTION('',(6.12323399569043E-17,-3.44926943328803E-17,1.00000000000003));
#3014=DIRECTION('',(0.963898423234107,-0.266270219301362,-6.82061332197052E-17));
#3015=DIRECTION('',(6.12323399569043E-17,-3.44926943328803E-17,1.00000000000003));
#3016=DIRECTION('',(0.963898423234107,-0.266270219301362,-6.82061332197052E-17));
#3017=DIRECTION('',(9.56752053399733E-17,3.25041224561462E-18,1.00000000000002));
#3018=DIRECTION('',(0.992607114562357,-0.121371809413001,-9.4573381092083E-17));
#3019=DIRECTION('',(9.56752053399733E-17,3.25041224561462E-18,1.00000000000002));
#3020=DIRECTION('',(0.992607114562357,-0.121371809413001,-9.4573381092083E-17));
#3021=DIRECTION('',(9.56752053399733E-17,3.25041224561462E-18,1.00000000000002));
#3022=DIRECTION('',(0.992607114562357,-0.121371809413001,-9.4573381092083E-17));
#3023=DIRECTION('',(9.56752053399733E-17,3.25041224561462E-18,1.00000000000002));
#3024=DIRECTION('',(0.992607114562357,-0.121371809413001,-9.4573381092083E-17));
#3025=DIRECTION('',(9.56752053399733E-17,3.25041224561462E-18,1.00000000000002));
#3026=DIRECTION('',(0.992607114562357,-0.121371809413001,-9.4573381092083E-17));
#3027=DIRECTION('',(9.56752053399733E-17,3.25041224561462E-18,1.00000000000002));
#3028=DIRECTION('',(0.992607114562357,-0.121371809413001,-9.4573381092083E-17));
#3029=CARTESIAN_POINT('',(0.,0.,0.));
#3030=CARTESIAN_POINT('',(0.,0.,0.));
#3031=CARTESIAN_POINT('Origin',(50.,-105.,5.));
#3032=CARTESIAN_POINT('',(45.5,-105.,10.));
#3033=CARTESIAN_POINT('Origin',(50.,-105.,10.));
#3034=CARTESIAN_POINT('',(45.5,-105.,0.));
#3035=CARTESIAN_POINT('',(45.5,-105.,5.));
#3036=CARTESIAN_POINT('Origin',(50.,-105.,0.));
#3037=CARTESIAN_POINT('Origin',(-20.,-105.,5.));
#3038=CARTESIAN_POINT('',(-24.5,-105.,10.));
#3039=CARTESIAN_POINT('Origin',(-20.,-105.,10.));
#3040=CARTESIAN_POINT('',(-24.5,-105.,0.));
#3041=CARTESIAN_POINT('',(-24.5,-105.,5.));
#3042=CARTESIAN_POINT('Origin',(-20.,-105.,0.));
#3043=CARTESIAN_POINT('Origin',(-20.,105.,5.));
#3044=CARTESIAN_POINT('',(-24.5,105.,10.));
#3045=CARTESIAN_POINT('Origin',(-20.,105.,10.));
#3046=CARTESIAN_POINT('',(-24.5,105.,0.));
#3047=CARTESIAN_POINT('',(-24.5,105.,5.));
#3048=CARTESIAN_POINT('Origin',(-20.,105.,0.));
#3049=CARTESIAN_POINT('Origin',(50.,105.,5.));
#3050=CARTESIAN_POINT('',(45.5,105.,10.));
#3051=CARTESIAN_POINT('Origin',(50.,105.,10.));
#3052=CARTESIAN_POINT('',(45.5,105.,0.));
#3053=CARTESIAN_POINT('',(45.5,105.,5.));
#3054=CARTESIAN_POINT('Origin',(50.,105.,0.));
#3055=CARTESIAN_POINT('Origin',(0.,0.,5.));
#3056=CARTESIAN_POINT('',(-5.,6.12323399573677E-16,10.));
#3057=CARTESIAN_POINT('Origin',(0.,0.,10.));
#3058=CARTESIAN_POINT('',(-5.,6.12323399573677E-16,0.));
#3059=CARTESIAN_POINT('',(-5.,6.12323399573677E-16,5.));
#3060=CARTESIAN_POINT('Origin',(0.,0.,0.));
#3061=CARTESIAN_POINT('Origin',(66.,125.,0.));
#3062=CARTESIAN_POINT('',(71.,125.,0.));
#3063=CARTESIAN_POINT('',(-39.,125.,0.));
#3064=CARTESIAN_POINT('',(41.,125.,0.));
#3065=CARTESIAN_POINT('',(-39.,125.,10.));
#3066=CARTESIAN_POINT('',(-39.,125.,0.));
#3067=CARTESIAN_POINT('',(71.,125.,10.));
#3068=CARTESIAN_POINT('',(41.,125.,10.));
#3069=CARTESIAN_POINT('',(71.,125.,0.));
#3070=CARTESIAN_POINT('Origin',(71.,-120.,0.));
#3071=CARTESIAN_POINT('',(71.,-125.,0.));
#3072=CARTESIAN_POINT('',(71.,-60.,0.));
#3073=CARTESIAN_POINT('',(71.,-125.,10.));
#3074=CARTESIAN_POINT('',(71.,-60.,10.));
#3075=CARTESIAN_POINT('',(71.,-125.,0.));
#3076=CARTESIAN_POINT('Origin',(-34.,-125.,0.));
#3077=CARTESIAN_POINT('',(-39.,-125.,0.));
#3078=CARTESIAN_POINT('',(-9.,-125.,0.));
#3079=CARTESIAN_POINT('',(-39.,-125.,10.));
#3080=CARTESIAN_POINT('',(-9.,-125.,10.));
#3081=CARTESIAN_POINT('',(-39.,-125.,0.));
#3082=CARTESIAN_POINT('Origin',(-39.,120.,0.));
#3083=CARTESIAN_POINT('',(-39.,60.,0.));
#3084=CARTESIAN_POINT('',(-39.,60.,10.));
#3085=CARTESIAN_POINT('Origin',(16.,0.,10.));
#3086=CARTESIAN_POINT('Origin',(16.,0.,0.));
#3087=CARTESIAN_POINT('',(0.,0.,0.));
#3088=CARTESIAN_POINT('Origin',(0.,0.,0.));
#3089=CARTESIAN_POINT('',(-5.,-6.12323399573677E-16,10.));
#3090=CARTESIAN_POINT('Origin',(0.,0.,10.));
#3091=CARTESIAN_POINT('',(-5.,-6.12323399573677E-16,0.));
#3092=CARTESIAN_POINT('',(-5.,-6.12323399573677E-16,0.));
#3093=CARTESIAN_POINT('Origin',(0.,0.,0.));
#3094=CARTESIAN_POINT('Origin',(0.,0.,0.));
#3095=CARTESIAN_POINT('',(-17.,2.0818995585505E-15,10.));
#3096=CARTESIAN_POINT('Origin',(0.,0.,10.));
#3097=CARTESIAN_POINT('',(-17.,2.0818995585505E-15,0.));
#3098=CARTESIAN_POINT('',(-17.,-2.0818995585505E-15,0.));
#3099=CARTESIAN_POINT('Origin',(0.,0.,0.));
#3100=CARTESIAN_POINT('Origin',(0.,0.,10.));
#3101=CARTESIAN_POINT('Origin',(0.,0.,0.));
#3102=CARTESIAN_POINT('',(0.,0.,0.));
#3103=CARTESIAN_POINT('Origin',(32.,0.,5.));
#3104=CARTESIAN_POINT('',(27.,6.12323399573677E-16,10.));
#3105=CARTESIAN_POINT('Origin',(32.,0.,10.));
#3106=CARTESIAN_POINT('',(27.,6.12323399573677E-16,0.));
#3107=CARTESIAN_POINT('',(27.,6.12323399573677E-16,5.));
#3108=CARTESIAN_POINT('Origin',(32.,0.,0.));
#3109=CARTESIAN_POINT('Origin',(52.,110.,0.));
#3110=CARTESIAN_POINT('',(52.,110.,0.));
#3111=CARTESIAN_POINT('',(12.,110.,0.));
#3112=CARTESIAN_POINT('',(52.,110.,0.));
#3113=CARTESIAN_POINT('',(12.,110.,10.));
#3114=CARTESIAN_POINT('',(12.,110.,0.));
#3115=CARTESIAN_POINT('',(52.,110.,10.));
#3116=CARTESIAN_POINT('',(52.,110.,10.));
#3117=CARTESIAN_POINT('',(52.,110.,0.));
#3118=CARTESIAN_POINT('Origin',(52.,-110.,0.));
#3119=CARTESIAN_POINT('',(52.,-110.,0.));
#3120=CARTESIAN_POINT('',(52.,-110.,0.));
#3121=CARTESIAN_POINT('',(52.,-110.,10.));
#3122=CARTESIAN_POINT('',(52.,-110.,10.));
#3123=CARTESIAN_POINT('',(52.,-110.,0.));
#3124=CARTESIAN_POINT('Origin',(12.,-110.,0.));
#3125=CARTESIAN_POINT('',(12.,-110.,0.));
#3126=CARTESIAN_POINT('',(12.,-110.,0.));
#3127=CARTESIAN_POINT('',(12.,-110.,10.));
#3128=CARTESIAN_POINT('',(12.,-110.,10.));
#3129=CARTESIAN_POINT('',(12.,-110.,0.));
#3130=CARTESIAN_POINT('Origin',(12.,110.,0.));
#3131=CARTESIAN_POINT('',(12.,110.,0.));
#3132=CARTESIAN_POINT('',(12.,110.,10.));
#3133=CARTESIAN_POINT('Origin',(32.,0.,10.));
#3134=CARTESIAN_POINT('Origin',(32.,0.,0.));
#3135=CARTESIAN_POINT('',(0.,0.,0.));
#3136=CARTESIAN_POINT('Origin',(0.,0.,4.));
#3137=CARTESIAN_POINT('',(-7.,8.57252759403147E-16,8.));
#3138=CARTESIAN_POINT('Origin',(0.,0.,8.));
#3139=CARTESIAN_POINT('',(-7.,8.57252759403147E-16,0.));
#3140=CARTESIAN_POINT('',(-7.,8.57252759403147E-16,4.));
#3141=CARTESIAN_POINT('Origin',(0.,0.,0.));
#3142=CARTESIAN_POINT('Origin',(32.,0.,4.));
#3143=CARTESIAN_POINT('',(25.,8.57252759403147E-16,8.));
#3144=CARTESIAN_POINT('Origin',(32.,0.,8.));
#3145=CARTESIAN_POINT('',(25.,8.57252759403147E-16,0.));
#3146=CARTESIAN_POINT('',(25.,8.57252759403147E-16,4.));
#3147=CARTESIAN_POINT('Origin',(32.,0.,0.));
#3148=CARTESIAN_POINT('Origin',(32.,12.,0.));
#3149=CARTESIAN_POINT('',(32.,12.,0.));
#3150=CARTESIAN_POINT('',(0.,12.,0.));
#3151=CARTESIAN_POINT('',(32.,12.,0.));
#3152=CARTESIAN_POINT('',(0.,12.,8.));
#3153=CARTESIAN_POINT('',(0.,12.,0.));
#3154=CARTESIAN_POINT('',(32.,12.,8.));
#3155=CARTESIAN_POINT('',(32.,12.,8.));
#3156=CARTESIAN_POINT('',(32.,12.,0.));
#3157=CARTESIAN_POINT('Origin',(32.,0.,0.));
#3158=CARTESIAN_POINT('',(32.,-12.,0.));
#3159=CARTESIAN_POINT('Origin',(32.,0.,0.));
#3160=CARTESIAN_POINT('',(32.,-12.,8.));
#3161=CARTESIAN_POINT('Origin',(32.,0.,8.));
#3162=CARTESIAN_POINT('',(32.,-12.,0.));
#3163=CARTESIAN_POINT('Origin',(0.,-12.,0.));
#3164=CARTESIAN_POINT('',(-1.46957615897682E-15,-12.,0.));
#3165=CARTESIAN_POINT('',(0.,-12.,0.));
#3166=CARTESIAN_POINT('',(-1.46957615897682E-15,-12.,8.));
#3167=CARTESIAN_POINT('',(0.,-12.,8.));
#3168=CARTESIAN_POINT('',(-1.46957615897682E-15,-12.,0.));
#3169=CARTESIAN_POINT('Origin',(0.,0.,0.));
#3170=CARTESIAN_POINT('Origin',(0.,0.,0.));
#3171=CARTESIAN_POINT('Origin',(0.,0.,8.));
#3172=CARTESIAN_POINT('Origin',(16.,0.,8.));
#3173=CARTESIAN_POINT('Origin',(16.,0.,0.));
#3174=CARTESIAN_POINT('',(0.,0.,0.));
#3175=CARTESIAN_POINT('Origin',(0.,0.,0.));
#3176=CARTESIAN_POINT('',(-8.,-9.79717439317883E-16,56.));
#3177=CARTESIAN_POINT('Origin',(0.,0.,56.));
#3178=CARTESIAN_POINT('',(-8.,-9.79717439317883E-16,0.));
#3179=CARTESIAN_POINT('',(-8.,-9.79717439317883E-16,0.));
#3180=CARTESIAN_POINT('Origin',(0.,0.,0.));
#3181=CARTESIAN_POINT('Origin',(0.,0.,56.));
#3182=CARTESIAN_POINT('Origin',(0.,0.,0.));
#3183=CARTESIAN_POINT('',(0.,0.,0.));
#3184=CARTESIAN_POINT('Origin',(0.,0.,4.));
#3185=CARTESIAN_POINT('',(-7.,8.57252759403147E-16,8.));
#3186=CARTESIAN_POINT('Origin',(0.,0.,8.));
#3187=CARTESIAN_POINT('',(-7.,8.57252759403147E-16,0.));
#3188=CARTESIAN_POINT('',(-7.,8.57252759403147E-16,4.));
#3189=CARTESIAN_POINT('Origin',(0.,0.,0.));
#3190=CARTESIAN_POINT('Origin',(100.,0.,4.));
#3191=CARTESIAN_POINT('',(93.,8.57252759403147E-16,8.));
#3192=CARTESIAN_POINT('Origin',(100.,0.,8.));
#3193=CARTESIAN_POINT('',(93.,8.57252759403147E-16,0.));
#3194=CARTESIAN_POINT('',(93.,8.57252759403147E-16,4.));
#3195=CARTESIAN_POINT('Origin',(100.,0.,0.));
#3196=CARTESIAN_POINT('Origin',(100.,12.,0.));
#3197=CARTESIAN_POINT('',(100.,12.,0.));
#3198=CARTESIAN_POINT('',(0.,12.,0.));
#3199=CARTESIAN_POINT('',(100.,12.,0.));
#3200=CARTESIAN_POINT('',(0.,12.,8.));
#3201=CARTESIAN_POINT('',(0.,12.,0.));
#3202=CARTESIAN_POINT('',(100.,12.,8.));
#3203=CARTESIAN_POINT('',(100.,12.,8.));
#3204=CARTESIAN_POINT('',(100.,12.,0.));
#3205=CARTESIAN_POINT('Origin',(100.,-1.11022302462516E-15,0.));
#3206=CARTESIAN_POINT('',(100.,-12.,0.));
#3207=CARTESIAN_POINT('Origin',(100.,-1.11022302462516E-15,0.));
#3208=CARTESIAN_POINT('',(100.,-12.,8.));
#3209=CARTESIAN_POINT('Origin',(100.,-1.11022302462516E-15,8.));
#3210=CARTESIAN_POINT('',(100.,-12.,0.));
#3211=CARTESIAN_POINT('Origin',(0.,-12.,0.));
#3212=CARTESIAN_POINT('',(-1.46957615897682E-15,-12.,0.));
#3213=CARTESIAN_POINT('',(0.,-12.,0.));
#3214=CARTESIAN_POINT('',(-1.46957615897682E-15,-12.,8.));
#3215=CARTESIAN_POINT('',(0.,-12.,8.));
#3216=CARTESIAN_POINT('',(-1.46957615897682E-15,-12.,0.));
#3217=CARTESIAN_POINT('Origin',(0.,0.,0.));
#3218=CARTESIAN_POINT('Origin',(0.,0.,0.));
#3219=CARTESIAN_POINT('Origin',(0.,0.,8.));
#3220=CARTESIAN_POINT('Origin',(50.,0.,8.));
#3221=CARTESIAN_POINT('Origin',(50.,0.,0.));
#3222=CARTESIAN_POINT('',(0.,0.,0.));
#3223=CARTESIAN_POINT('Origin',(0.,0.,4.));
#3224=CARTESIAN_POINT('',(-7.,8.57252759403147E-16,8.));
#3225=CARTESIAN_POINT('Origin',(0.,0.,8.));
#3226=CARTESIAN_POINT('',(-7.,8.57252759403147E-16,0.));
#3227=CARTESIAN_POINT('',(-7.,8.57252759403147E-16,4.));
#3228=CARTESIAN_POINT('Origin',(0.,0.,0.));
#3229=CARTESIAN_POINT('Origin',(60.,0.,4.));
#3230=CARTESIAN_POINT('',(53.,8.57252759403147E-16,8.));
#3231=CARTESIAN_POINT('Origin',(60.,0.,8.));
#3232=CARTESIAN_POINT('',(53.,8.57252759403147E-16,0.));
#3233=CARTESIAN_POINT('',(53.,8.57252759403147E-16,4.));
#3234=CARTESIAN_POINT('Origin',(60.,0.,0.));
#3235=CARTESIAN_POINT('Origin',(60.,12.,0.));
#3236=CARTESIAN_POINT('',(60.,12.,0.));
#3237=CARTESIAN_POINT('',(0.,12.,0.));
#3238=CARTESIAN_POINT('',(60.,12.,0.));
#3239=CARTESIAN_POINT('',(0.,12.,8.));
#3240=CARTESIAN_POINT('',(0.,12.,0.));
#3241=CARTESIAN_POINT('',(60.,12.,8.));
#3242=CARTESIAN_POINT('',(60.,12.,8.));
#3243=CARTESIAN_POINT('',(60.,12.,0.));
#3244=CARTESIAN_POINT('Origin',(60.,0.,0.));
#3245=CARTESIAN_POINT('',(60.,-12.,0.));
#3246=CARTESIAN_POINT('Origin',(60.,0.,0.));
#3247=CARTESIAN_POINT('',(60.,-12.,8.));
#3248=CARTESIAN_POINT('Origin',(60.,0.,8.));
#3249=CARTESIAN_POINT('',(60.,-12.,0.));
#3250=CARTESIAN_POINT('Origin',(0.,-12.,0.));
#3251=CARTESIAN_POINT('',(-1.46957615897682E-15,-12.,0.));
#3252=CARTESIAN_POINT('',(0.,-12.,0.));
#3253=CARTESIAN_POINT('',(-1.46957615897682E-15,-12.,8.));
#3254=CARTESIAN_POINT('',(0.,-12.,8.));
#3255=CARTESIAN_POINT('',(-1.46957615897682E-15,-12.,0.));
#3256=CARTESIAN_POINT('Origin',(0.,0.,0.));
#3257=CARTESIAN_POINT('Origin',(0.,0.,0.));
#3258=CARTESIAN_POINT('Origin',(0.,0.,8.));
#3259=CARTESIAN_POINT('Origin',(30.,0.,8.));
#3260=CARTESIAN_POINT('Origin',(30.,0.,0.));
#3261=CARTESIAN_POINT('',(0.,0.,0.));
#3262=CARTESIAN_POINT('Origin',(0.,0.,39.));
#3263=CARTESIAN_POINT('',(-4.,-4.89858719658941E-16,38.));
#3264=CARTESIAN_POINT('Origin',(0.,0.,38.));
#3265=CARTESIAN_POINT('',(-4.,-4.89858719658941E-16,40.));
#3266=CARTESIAN_POINT('',(-4.,-4.89858719658941E-16,39.));
#3267=CARTESIAN_POINT('Origin',(0.,0.,40.));
#3268=CARTESIAN_POINT('Origin',(8.,0.,38.));
#3269=CARTESIAN_POINT('',(-5.,6.12323399573677E-16,38.));
#3270=CARTESIAN_POINT('Origin',(0.,0.,38.));
#3271=CARTESIAN_POINT('Origin',(4.,0.,40.));
#3272=CARTESIAN_POINT('',(-5.,-6.12323399573677E-16,40.));
#3273=CARTESIAN_POINT('Origin',(0.,0.,40.));
#3274=CARTESIAN_POINT('Origin',(0.,0.,0.));
#3275=CARTESIAN_POINT('',(-5.,-6.12323399573677E-16,41.));
#3276=CARTESIAN_POINT('Origin',(0.,0.,41.));
#3277=CARTESIAN_POINT('',(-5.,-6.12323399573677E-16,0.));
#3278=CARTESIAN_POINT('Origin',(0.,0.,0.));
#3279=CARTESIAN_POINT('',(-8.,-9.79717439317883E-16,0.));
#3280=CARTESIAN_POINT('Origin',(0.,0.,0.));
#3281=CARTESIAN_POINT('',(-5.,-6.12323399573677E-16,0.));
#3282=CARTESIAN_POINT('Origin',(0.,0.,0.));
#3283=CARTESIAN_POINT('Origin',(0.,0.,-4.));
#3284=CARTESIAN_POINT('',(-8.,-9.79717439317883E-16,-4.));
#3285=CARTESIAN_POINT('',(-8.,-9.79717439317883E-16,-4.));
#3286=CARTESIAN_POINT('Origin',(0.,0.,-4.));
#3287=CARTESIAN_POINT('Origin',(0.,0.,-4.));
#3288=CARTESIAN_POINT('Origin',(0.,0.,0.));
#3289=CARTESIAN_POINT('',(-5.,-6.12323399573677E-16,0.));
#3290=CARTESIAN_POINT('Origin',(0.,0.,41.));
#3291=CARTESIAN_POINT('',(0.,0.,0.));
#3292=CARTESIAN_POINT('Origin',(0.,0.,27.));
#3293=CARTESIAN_POINT('',(-4.,-4.89858719658941E-16,26.));
#3294=CARTESIAN_POINT('Origin',(0.,0.,26.));
#3295=CARTESIAN_POINT('',(-4.,-4.89858719658941E-16,28.));
#3296=CARTESIAN_POINT('',(-4.,-4.89858719658941E-16,27.));
#3297=CARTESIAN_POINT('Origin',(0.,0.,28.));
#3298=CARTESIAN_POINT('Origin',(8.,0.,26.));
#3299=CARTESIAN_POINT('',(-5.,6.12323399573677E-16,26.));
#3300=CARTESIAN_POINT('Origin',(0.,0.,26.));
#3301=CARTESIAN_POINT('Origin',(4.,0.,28.));
#3302=CARTESIAN_POINT('',(-5.,-6.12323399573677E-16,28.));
#3303=CARTESIAN_POINT('Origin',(0.,0.,28.));
#3304=CARTESIAN_POINT('Origin',(0.,0.,0.));
#3305=CARTESIAN_POINT('',(-5.,-6.12323399573677E-16,29.));
#3306=CARTESIAN_POINT('Origin',(0.,0.,29.));
#3307=CARTESIAN_POINT('',(-5.,-6.12323399573677E-16,0.));
#3308=CARTESIAN_POINT('Origin',(0.,0.,0.));
#3309=CARTESIAN_POINT('',(-8.,-9.79717439317883E-16,0.));
#3310=CARTESIAN_POINT('Origin',(0.,0.,0.));
#3311=CARTESIAN_POINT('',(-5.,-6.12323399573677E-16,0.));
#3312=CARTESIAN_POINT('Origin',(0.,0.,0.));
#3313=CARTESIAN_POINT('Origin',(0.,0.,-4.));
#3314=CARTESIAN_POINT('',(-8.,-9.79717439317883E-16,-4.));
#3315=CARTESIAN_POINT('',(-8.,-9.79717439317883E-16,-4.));
#3316=CARTESIAN_POINT('Origin',(0.,0.,-4.));
#3317=CARTESIAN_POINT('Origin',(0.,0.,-4.));
#3318=CARTESIAN_POINT('Origin',(0.,0.,0.));
#3319=CARTESIAN_POINT('',(-5.,-6.12323399573677E-16,0.));
#3320=CARTESIAN_POINT('Origin',(0.,0.,29.));
#3321=CARTESIAN_POINT('',(0.,0.,0.));
#3322=CARTESIAN_POINT('Origin',(0.,0.,0.));
#3323=CARTESIAN_POINT('',(-5.,-6.12323399573677E-16,6.));
#3324=CARTESIAN_POINT('Origin',(0.,0.,6.));
#3325=CARTESIAN_POINT('',(-5.,-6.12323399573677E-16,0.));
#3326=CARTESIAN_POINT('',(-5.,-6.12323399573677E-16,0.));
#3327=CARTESIAN_POINT('Origin',(0.,0.,0.));
#3328=CARTESIAN_POINT('Origin',(0.,0.,0.));
#3329=CARTESIAN_POINT('',(-7.,-8.57252759403147E-16,6.));
#3330=CARTESIAN_POINT('Origin',(0.,0.,6.));
#3331=CARTESIAN_POINT('',(-7.,-8.57252759403147E-16,0.));
#3332=CARTESIAN_POINT('',(-7.,-8.57252759403147E-16,0.));
#3333=CARTESIAN_POINT('Origin',(0.,0.,0.));
#3334=CARTESIAN_POINT('Origin',(0.,0.,6.));
#3335=CARTESIAN_POINT('Origin',(0.,0.,0.));
#3336=CARTESIAN_POINT('',(0.,0.,0.));
#3337=CARTESIAN_POINT('Origin',(0.,0.,45.));
#3338=CARTESIAN_POINT('',(-4.,-4.89858719658941E-16,44.));
#3339=CARTESIAN_POINT('Origin',(0.,0.,44.));
#3340=CARTESIAN_POINT('',(-4.,-4.89858719658941E-16,46.));
#3341=CARTESIAN_POINT('',(-4.,-4.89858719658941E-16,45.));
#3342=CARTESIAN_POINT('Origin',(0.,0.,46.));
#3343=CARTESIAN_POINT('Origin',(8.,0.,44.));
#3344=CARTESIAN_POINT('',(-5.,6.12323399573677E-16,44.));
#3345=CARTESIAN_POINT('Origin',(0.,0.,44.));
#3346=CARTESIAN_POINT('Origin',(4.,0.,46.));
#3347=CARTESIAN_POINT('',(-5.,-6.12323399573677E-16,46.));
#3348=CARTESIAN_POINT('Origin',(0.,0.,46.));
#3349=CARTESIAN_POINT('Origin',(0.,0.,0.));
#3350=CARTESIAN_POINT('',(-5.,-6.12323399573677E-16,47.));
#3351=CARTESIAN_POINT('Origin',(0.,0.,47.));
#3352=CARTESIAN_POINT('',(-5.,-6.12323399573677E-16,0.));
#3353=CARTESIAN_POINT('Origin',(0.,0.,0.));
#3354=CARTESIAN_POINT('',(-8.,-9.79717439317883E-16,0.));
#3355=CARTESIAN_POINT('Origin',(0.,0.,0.));
#3356=CARTESIAN_POINT('',(-5.,-6.12323399573677E-16,0.));
#3357=CARTESIAN_POINT('Origin',(0.,0.,0.));
#3358=CARTESIAN_POINT('Origin',(0.,0.,-2.));
#3359=CARTESIAN_POINT('',(-8.,-9.79717439317883E-16,-2.));
#3360=CARTESIAN_POINT('',(-8.,-9.79717439317883E-16,-2.));
#3361=CARTESIAN_POINT('Origin',(0.,0.,-2.));
#3362=CARTESIAN_POINT('Origin',(0.,0.,-2.));
#3363=CARTESIAN_POINT('',(-2.,-2.44929359829471E-16,-2.));
#3364=CARTESIAN_POINT('Origin',(0.,0.,-2.));
#3365=CARTESIAN_POINT('Origin',(0.,0.,0.));
#3366=CARTESIAN_POINT('',(-2.,-2.44929359829471E-16,47.));
#3367=CARTESIAN_POINT('Origin',(0.,0.,47.));
#3368=CARTESIAN_POINT('',(-2.,-2.44929359829471E-16,0.));
#3369=CARTESIAN_POINT('Origin',(0.,0.,0.));
#3370=CARTESIAN_POINT('',(-5.,-6.12323399573677E-16,0.));
#3371=CARTESIAN_POINT('Origin',(0.,0.,47.));
#3372=CARTESIAN_POINT('',(0.,0.,0.));
#3373=CARTESIAN_POINT('Origin',(0.,0.,0.));
#3374=CARTESIAN_POINT('',(-5.,-6.12323399573677E-16,8.));
#3375=CARTESIAN_POINT('Origin',(0.,0.,8.));
#3376=CARTESIAN_POINT('',(-5.,-6.12323399573677E-16,0.));
#3377=CARTESIAN_POINT('',(-5.,-6.12323399573677E-16,0.));
#3378=CARTESIAN_POINT('Origin',(0.,0.,0.));
#3379=CARTESIAN_POINT('Origin',(0.,0.,0.));
#3380=CARTESIAN_POINT('',(-7.,-8.57252759403147E-16,8.));
#3381=CARTESIAN_POINT('Origin',(0.,0.,8.));
#3382=CARTESIAN_POINT('',(-7.,-8.57252759403147E-16,0.));
#3383=CARTESIAN_POINT('',(-7.,-8.57252759403147E-16,0.));
#3384=CARTESIAN_POINT('Origin',(0.,0.,0.));
#3385=CARTESIAN_POINT('Origin',(0.,0.,8.));
#3386=CARTESIAN_POINT('Origin',(0.,0.,0.));
#3387=CARTESIAN_POINT('',(0.,0.,0.));
#3388=CARTESIAN_POINT('Origin',(0.,0.,4.));
#3389=CARTESIAN_POINT('',(-2.,-2.44929359829471E-16,80.));
#3390=CARTESIAN_POINT('Origin',(0.,0.,80.));
#3391=CARTESIAN_POINT('',(-2.,-2.44929359829471E-16,4.));
#3392=CARTESIAN_POINT('',(-2.,-2.44929359829471E-16,4.));
#3393=CARTESIAN_POINT('Origin',(0.,0.,4.));
#3394=CARTESIAN_POINT('Origin',(0.,0.,80.));
#3395=CARTESIAN_POINT('Origin',(0.,0.,2.));
#3396=CARTESIAN_POINT('',(0.,0.,0.));
#3397=CARTESIAN_POINT('',(-1.,-1.22464679914735E-16,2.));
#3398=CARTESIAN_POINT('',(0.,0.,0.));
#3399=CARTESIAN_POINT('Origin',(0.,0.,45.));
#3400=CARTESIAN_POINT('',(-4.,-4.89858719658941E-16,44.));
#3401=CARTESIAN_POINT('Origin',(0.,0.,44.));
#3402=CARTESIAN_POINT('',(-4.,-4.89858719658941E-16,46.));
#3403=CARTESIAN_POINT('',(-4.,-4.89858719658941E-16,45.));
#3404=CARTESIAN_POINT('Origin',(0.,0.,46.));
#3405=CARTESIAN_POINT('Origin',(8.,0.,44.));
#3406=CARTESIAN_POINT('',(-5.,6.12323399573677E-16,44.));
#3407=CARTESIAN_POINT('Origin',(0.,0.,44.));
#3408=CARTESIAN_POINT('Origin',(4.,0.,46.));
#3409=CARTESIAN_POINT('',(-5.,-6.12323399573677E-16,46.));
#3410=CARTESIAN_POINT('Origin',(0.,0.,46.));
#3411=CARTESIAN_POINT('Origin',(0.,0.,0.));
#3412=CARTESIAN_POINT('',(-5.,-6.12323399573677E-16,47.));
#3413=CARTESIAN_POINT('Origin',(0.,0.,47.));
#3414=CARTESIAN_POINT('',(-5.,-6.12323399573677E-16,0.));
#3415=CARTESIAN_POINT('Origin',(0.,0.,0.));
#3416=CARTESIAN_POINT('',(-8.,-9.79717439317883E-16,0.));
#3417=CARTESIAN_POINT('Origin',(0.,0.,0.));
#3418=CARTESIAN_POINT('',(-5.,-6.12323399573677E-16,0.));
#3419=CARTESIAN_POINT('Origin',(0.,0.,0.));
#3420=CARTESIAN_POINT('Origin',(0.,0.,-2.));
#3421=CARTESIAN_POINT('',(-8.,-9.79717439317883E-16,-2.));
#3422=CARTESIAN_POINT('',(-8.,-9.79717439317883E-16,-2.));
#3423=CARTESIAN_POINT('Origin',(0.,0.,-2.));
#3424=CARTESIAN_POINT('Origin',(0.,0.,-2.));
#3425=CARTESIAN_POINT('Origin',(0.,0.,0.));
#3426=CARTESIAN_POINT('',(-5.,-6.12323399573677E-16,0.));
#3427=CARTESIAN_POINT('Origin',(0.,0.,47.));
#3428=CARTESIAN_POINT('',(0.,0.,0.));
#3429=CARTESIAN_POINT('Origin',(0.,0.,0.));
#3430=CARTESIAN_POINT('',(-5.,-6.12323399573677E-16,8.));
#3431=CARTESIAN_POINT('Origin',(0.,0.,8.));
#3432=CARTESIAN_POINT('',(-5.,-6.12323399573677E-16,0.));
#3433=CARTESIAN_POINT('',(-5.,-6.12323399573677E-16,0.));
#3434=CARTESIAN_POINT('Origin',(0.,0.,0.));
#3435=CARTESIAN_POINT('Origin',(0.,0.,0.));
#3436=CARTESIAN_POINT('',(-7.,-8.57252759403147E-16,8.));
#3437=CARTESIAN_POINT('Origin',(0.,0.,8.));
#3438=CARTESIAN_POINT('',(-7.,-8.57252759403147E-16,0.));
#3439=CARTESIAN_POINT('',(-7.,-8.57252759403147E-16,0.));
#3440=CARTESIAN_POINT('Origin',(0.,0.,0.));
#3441=CARTESIAN_POINT('Origin',(0.,0.,8.));
#3442=CARTESIAN_POINT('Origin',(0.,0.,0.));
#3443=CARTESIAN_POINT('',(0.,0.,0.));
#3444=CARTESIAN_POINT('Origin',(0.,0.,0.));
#3445=CARTESIAN_POINT('',(-5.,-6.12323399573677E-16,2.));
#3446=CARTESIAN_POINT('Origin',(0.,0.,2.));
#3447=CARTESIAN_POINT('',(-5.,-6.12323399573677E-16,0.));
#3448=CARTESIAN_POINT('',(-5.,-6.12323399573677E-16,0.));
#3449=CARTESIAN_POINT('Origin',(0.,0.,0.));
#3450=CARTESIAN_POINT('Origin',(0.,0.,0.));
#3451=CARTESIAN_POINT('',(-10.,-1.22464679914735E-15,2.));
#3452=CARTESIAN_POINT('Origin',(0.,0.,2.));
#3453=CARTESIAN_POINT('',(-10.,-1.22464679914735E-15,0.));
#3454=CARTESIAN_POINT('',(-10.,-1.22464679914735E-15,0.));
#3455=CARTESIAN_POINT('Origin',(0.,0.,0.));
#3456=CARTESIAN_POINT('Origin',(0.,0.,2.));
#3457=CARTESIAN_POINT('Origin',(0.,0.,0.));
#3458=CARTESIAN_POINT('',(0.,0.,0.));
#3459=CARTESIAN_POINT('Origin',(-1.,0.,1.));
#3460=CARTESIAN_POINT('',(-1.,3.87298334620742,0.));
#3461=CARTESIAN_POINT('',(-1.,3.87298334620742,1.));
#3462=CARTESIAN_POINT('',(-1.,3.87298334620742,0.));
#3463=CARTESIAN_POINT('',(-1.,7.93725393319377,0.));
#3464=CARTESIAN_POINT('',(-1.,0.,0.));
#3465=CARTESIAN_POINT('',(-1.,7.93725393319377,1.));
#3466=CARTESIAN_POINT('',(-1.,7.93725393319377,0.));
#3467=CARTESIAN_POINT('',(-1.,0.,1.));
#3468=CARTESIAN_POINT('Origin',(1.,16.,1.));
#3469=CARTESIAN_POINT('',(1.,3.87298334620742,1.));
#3470=CARTESIAN_POINT('',(1.,3.87298334620742,0.));
#3471=CARTESIAN_POINT('',(1.,3.87298334620742,0.));
#3472=CARTESIAN_POINT('',(1.,7.93725393319377,1.));
#3473=CARTESIAN_POINT('',(1.,8.,1.));
#3474=CARTESIAN_POINT('',(1.,7.93725393319377,0.));
#3475=CARTESIAN_POINT('',(1.,7.93725393319377,0.));
#3476=CARTESIAN_POINT('',(1.,8.,0.));
#3477=CARTESIAN_POINT('Origin',(0.,0.,0.));
#3478=CARTESIAN_POINT('Origin',(0.,0.,0.));
#3479=CARTESIAN_POINT('Origin',(0.,0.,0.));
#3480=CARTESIAN_POINT('Origin',(0.,0.,0.));
#3481=CARTESIAN_POINT('Origin',(0.,0.,1.));
#3482=CARTESIAN_POINT('Origin',(0.,0.,0.));
#3483=CARTESIAN_POINT('Origin',(0.,0.,1.));
#3484=CARTESIAN_POINT('Origin',(0.,0.,1.));
#3485=CARTESIAN_POINT('',(0.,0.,0.));
#3486=CARTESIAN_POINT('',(0.,0.,10.));
#3487=CARTESIAN_POINT('',(32.,-100.,10.));
#3488=CARTESIAN_POINT('',(0.,0.,66.));
#3489=CARTESIAN_POINT('',(-2.72943971527439E-15,-4.41534177390351E-15,19.9999999999998));
#3490=CARTESIAN_POINT('',(89.0799515546372,45.4396548294966,36.0000000000002));
#3491=CARTESIAN_POINT('',(32.,4.85722573273506E-16,52.0000000000006));
#3492=CARTESIAN_POINT('',(1.97423192444653E-14,2.83373964276182E-14,19.9999999999998));
#3493=CARTESIAN_POINT('',(32.,100.,10.));
#3494=CARTESIAN_POINT('',(-1.84193262457468E-15,-3.57932622488482E-16,28.));
#3495=CARTESIAN_POINT('',(73.7647979888567,-67.5185498782623,44.0000000000004));
#3496=CARTESIAN_POINT('',(89.0799515546372,45.4396548294965,44.0000000000003));
#3497=CARTESIAN_POINT('',(73.7647979888567,-67.5185498782623,36.0000000000001));
#3498=CARTESIAN_POINT('',(0.,0.,0.));
#3499=CARTESIAN_POINT('',(32.,0.,76.));
#3500=CARTESIAN_POINT('',(32.,0.,60.));
#3501=CARTESIAN_POINT('',(89.0799515546372,45.4396548294966,17.9999999999998));
#3502=CARTESIAN_POINT('',(100.000000000002,-13.558248031122,18.));
#3503=CARTESIAN_POINT('',(89.0799515546373,45.4396548294965,27.9999999999999));
#3504=CARTESIAN_POINT('',(0.,0.,36.));
#3505=CARTESIAN_POINT('',(89.0799515546372,45.4396548294966,19.9999999999998));
#3506=CARTESIAN_POINT('',(-5.11677153243246E-14,3.30612420314686E-14,28.));
#3507=CARTESIAN_POINT('',(73.7647979888567,-67.5185498782623,28.));
#3508=CARTESIAN_POINT('',(89.0799515546373,45.4396548294965,36.0000000000002));
#3509=CARTESIAN_POINT('',(62.8447495434919,-8.52064701764391,36.0000000000002));
#3510=CARTESIAN_POINT('',(73.7647979888567,-67.5185498782622,44.0000000000004));
#3511=CARTESIAN_POINT('',(62.8447495434921,-8.52064701764368,44.0000000000004));
#3512=CARTESIAN_POINT('',(89.0799515546372,45.4396548294965,44.0000000000003));
#3513=CARTESIAN_POINT('',(100.000000000002,-13.558248031122,44.0000000000003));
#3514=CARTESIAN_POINT('',(73.7647979888566,-67.5185498782623,36.0000000000001));
#3515=CARTESIAN_POINT('',(100.000000000001,-13.5582480311218,36.0000000000001));
#3516=CARTESIAN_POINT('',(32.,4.85722573273506E-16,52.0000000000006));
#3517=CARTESIAN_POINT('',(62.844749543492,-8.52064701764376,52.0000000000006));
#3518=CARTESIAN_POINT('',(0.,0.,39.));
#3519=CARTESIAN_POINT('',(100.000000000002,-13.558248031122,-4.1552406203209E-13));
#3520=CARTESIAN_POINT('',(32.,0.,50.));
#3521=CARTESIAN_POINT('',(32.,0.,48.));
#3522=CARTESIAN_POINT('',(89.0799515546372,45.4396548294966,52.0000000000004));
#3523=CARTESIAN_POINT('',(89.0799515546372,45.4396548294966,17.9999999999998));
#3524=CARTESIAN_POINT('',(89.0799515546372,45.4396548294966,60.0000000000013));
#3525=CARTESIAN_POINT('',(89.0799515546372,45.4396548294967,63.0000000000013));
#3526=CARTESIAN_POINT('',(73.7647979888567,-67.5185498782623,18.));
#3527=CARTESIAN_POINT('',(73.7647979888567,-67.5185498782623,20.));
#3528=CARTESIAN_POINT('',(73.7647979888568,-67.5185498782623,52.0000000000006));
#3529=CARTESIAN_POINT('',(73.7647979888567,-67.5185498782623,18.));
#3530=CARTESIAN_POINT('',(73.7647979888568,-67.5185498782624,60.0000000000013));
#3531=CARTESIAN_POINT('',(73.7647979888569,-67.5185498782624,63.0000000000013));
#3532=CARTESIAN_POINT('',(62.844749543492,-8.52064701764377,18.));
#3533=CARTESIAN_POINT('',(62.844749543492,-8.52064701764377,20.));
#3534=CARTESIAN_POINT('',(62.844749543492,-8.52064701764376,28.));
#3535=CARTESIAN_POINT('',(62.844749543492,-8.52064701764377,18.));
#3536=CARTESIAN_POINT('',(62.844749543492,-8.52064701764376,60.0000000000015));
#3537=CARTESIAN_POINT('',(62.844749543492,-8.52064701764378,63.0000000000015));
#3538=CARTESIAN_POINT('',(100.000000000002,-13.558248031122,20.));
#3539=CARTESIAN_POINT('',(100.000000000002,-13.558248031122,28.));
#3540=CARTESIAN_POINT('',(100.000000000002,-13.558248031122,52.0000000000004));
#3541=CARTESIAN_POINT('',(100.000000000002,-13.558248031122,18.));
#3542=CARTESIAN_POINT('',(100.000000000002,-13.558248031122,60.0000000000012));
#3543=CARTESIAN_POINT('',(100.000000000002,-13.558248031122,63.0000000000013));
#3544=UNCERTAINTY_MEASURE_WITH_UNIT(LENGTH_MEASURE(0.01),#3582,
'DISTANCE_ACCURACY_VALUE',
'Maximum model space distance between geometric entities at asserted c
onnectivities');
#3545=UNCERTAINTY_MEASURE_WITH_UNIT(LENGTH_MEASURE(0.01),#3582,
'DISTANCE_ACCURACY_VALUE',
'Maximum model space distance between geometric entities at asserted c
onnectivities');
#3546=UNCERTAINTY_MEASURE_WITH_UNIT(LENGTH_MEASURE(0.01),#3582,
'DISTANCE_ACCURACY_VALUE',
'Maximum model space distance between geometric entities at asserted c
onnectivities');
#3547=UNCERTAINTY_MEASURE_WITH_UNIT(LENGTH_MEASURE(0.01),#3582,
'DISTANCE_ACCURACY_VALUE',
'Maximum model space distance between geometric entities at asserted c
onnectivities');
#3548=UNCERTAINTY_MEASURE_WITH_UNIT(LENGTH_MEASURE(0.01),#3582,
'DISTANCE_ACCURACY_VALUE',
'Maximum model space distance between geometric entities at asserted c
onnectivities');
#3549=UNCERTAINTY_MEASURE_WITH_UNIT(LENGTH_MEASURE(0.01),#3582,
'DISTANCE_ACCURACY_VALUE',
'Maximum model space distance between geometric entities at asserted c
onnectivities');
#3550=UNCERTAINTY_MEASURE_WITH_UNIT(LENGTH_MEASURE(0.01),#3582,
'DISTANCE_ACCURACY_VALUE',
'Maximum model space distance between geometric entities at asserted c
onnectivities');
#3551=UNCERTAINTY_MEASURE_WITH_UNIT(LENGTH_MEASURE(0.01),#3582,
'DISTANCE_ACCURACY_VALUE',
'Maximum model space distance between geometric entities at asserted c
onnectivities');
#3552=UNCERTAINTY_MEASURE_WITH_UNIT(LENGTH_MEASURE(0.01),#3582,
'DISTANCE_ACCURACY_VALUE',
'Maximum model space distance between geometric entities at asserted c
onnectivities');
#3553=UNCERTAINTY_MEASURE_WITH_UNIT(LENGTH_MEASURE(0.01),#3582,
'DISTANCE_ACCURACY_VALUE',
'Maximum model space distance between geometric entities at asserted c
onnectivities');
#3554=UNCERTAINTY_MEASURE_WITH_UNIT(LENGTH_MEASURE(0.01),#3582,
'DISTANCE_ACCURACY_VALUE',
'Maximum model space distance between geometric entities at asserted c
onnectivities');
#3555=UNCERTAINTY_MEASURE_WITH_UNIT(LENGTH_MEASURE(0.01),#3582,
'DISTANCE_ACCURACY_VALUE',
'Maximum model space distance between geometric entities at asserted c
onnectivities');
#3556=UNCERTAINTY_MEASURE_WITH_UNIT(LENGTH_MEASURE(0.01),#3582,
'DISTANCE_ACCURACY_VALUE',
'Maximum model space distance between geometric entities at asserted c
onnectivities');
#3557=UNCERTAINTY_MEASURE_WITH_UNIT(LENGTH_MEASURE(0.01),#3582,
'DISTANCE_ACCURACY_VALUE',
'Maximum model space distance between geometric entities at asserted c
onnectivities');
#3558=UNCERTAINTY_MEASURE_WITH_UNIT(LENGTH_MEASURE(0.01),#3582,
'DISTANCE_ACCURACY_VALUE',
'Maximum model space distance between geometric entities at asserted c
onnectivities');
#3559=UNCERTAINTY_MEASURE_WITH_UNIT(LENGTH_MEASURE(0.01),#3582,
'DISTANCE_ACCURACY_VALUE',
'Maximum model space distance between geometric entities at asserted c
onnectivities');
#3560=UNCERTAINTY_MEASURE_WITH_UNIT(LENGTH_MEASURE(0.01),#3582,
'DISTANCE_ACCURACY_VALUE',
'Maximum model space distance between geometric entities at asserted c
onnectivities');
#3561=UNCERTAINTY_MEASURE_WITH_UNIT(LENGTH_MEASURE(0.01),#3582,
'DISTANCE_ACCURACY_VALUE',
'Maximum model space distance between geometric entities at asserted c
onnectivities');
#3562=UNCERTAINTY_MEASURE_WITH_UNIT(LENGTH_MEASURE(0.01),#3582,
'DISTANCE_ACCURACY_VALUE',
'Maximum model space distance between geometric entities at asserted c
onnectivities');
#3563=(
GEOMETRIC_REPRESENTATION_CONTEXT(3)
GLOBAL_UNCERTAINTY_ASSIGNED_CONTEXT((#3544))
GLOBAL_UNIT_ASSIGNED_CONTEXT((#3582,#3584,#3585))
REPRESENTATION_CONTEXT('','3D')
);
#3564=(
GEOMETRIC_REPRESENTATION_CONTEXT(3)
GLOBAL_UNCERTAINTY_ASSIGNED_CONTEXT((#3545))
GLOBAL_UNIT_ASSIGNED_CONTEXT((#3582,#3584,#3585))
REPRESENTATION_CONTEXT('','3D')
);
#3565=(
GEOMETRIC_REPRESENTATION_CONTEXT(3)
GLOBAL_UNCERTAINTY_ASSIGNED_CONTEXT((#3546))
GLOBAL_UNIT_ASSIGNED_CONTEXT((#3582,#3584,#3585))
REPRESENTATION_CONTEXT('','3D')
);
#3566=(
GEOMETRIC_REPRESENTATION_CONTEXT(3)
GLOBAL_UNCERTAINTY_ASSIGNED_CONTEXT((#3547))
GLOBAL_UNIT_ASSIGNED_CONTEXT((#3582,#3584,#3585))
REPRESENTATION_CONTEXT('','3D')
);
#3567=(
GEOMETRIC_REPRESENTATION_CONTEXT(3)
GLOBAL_UNCERTAINTY_ASSIGNED_CONTEXT((#3548))
GLOBAL_UNIT_ASSIGNED_CONTEXT((#3582,#3584,#3585))
REPRESENTATION_CONTEXT('','3D')
);
#3568=(
GEOMETRIC_REPRESENTATION_CONTEXT(3)
GLOBAL_UNCERTAINTY_ASSIGNED_CONTEXT((#3549))
GLOBAL_UNIT_ASSIGNED_CONTEXT((#3582,#3584,#3585))
REPRESENTATION_CONTEXT('','3D')
);
#3569=(
GEOMETRIC_REPRESENTATION_CONTEXT(3)
GLOBAL_UNCERTAINTY_ASSIGNED_CONTEXT((#3550))
GLOBAL_UNIT_ASSIGNED_CONTEXT((#3582,#3584,#3585))
REPRESENTATION_CONTEXT('','3D')
);
#3570=(
GEOMETRIC_REPRESENTATION_CONTEXT(3)
GLOBAL_UNCERTAINTY_ASSIGNED_CONTEXT((#3551))
GLOBAL_UNIT_ASSIGNED_CONTEXT((#3582,#3584,#3585))
REPRESENTATION_CONTEXT('','3D')
);
#3571=(
GEOMETRIC_REPRESENTATION_CONTEXT(3)
GLOBAL_UNCERTAINTY_ASSIGNED_CONTEXT((#3552))
GLOBAL_UNIT_ASSIGNED_CONTEXT((#3582,#3584,#3585))
REPRESENTATION_CONTEXT('','3D')
);
#3572=(
GEOMETRIC_REPRESENTATION_CONTEXT(3)
GLOBAL_UNCERTAINTY_ASSIGNED_CONTEXT((#3553))
GLOBAL_UNIT_ASSIGNED_CONTEXT((#3582,#3584,#3585))
REPRESENTATION_CONTEXT('','3D')
);
#3573=(
GEOMETRIC_REPRESENTATION_CONTEXT(3)
GLOBAL_UNCERTAINTY_ASSIGNED_CONTEXT((#3554))
GLOBAL_UNIT_ASSIGNED_CONTEXT((#3582,#3584,#3585))
REPRESENTATION_CONTEXT('','3D')
);
#3574=(
GEOMETRIC_REPRESENTATION_CONTEXT(3)
GLOBAL_UNCERTAINTY_ASSIGNED_CONTEXT((#3555))
GLOBAL_UNIT_ASSIGNED_CONTEXT((#3582,#3584,#3585))
REPRESENTATION_CONTEXT('','3D')
);
#3575=(
GEOMETRIC_REPRESENTATION_CONTEXT(3)
GLOBAL_UNCERTAINTY_ASSIGNED_CONTEXT((#3556))
GLOBAL_UNIT_ASSIGNED_CONTEXT((#3582,#3584,#3585))
REPRESENTATION_CONTEXT('','3D')
);
#3576=(
GEOMETRIC_REPRESENTATION_CONTEXT(3)
GLOBAL_UNCERTAINTY_ASSIGNED_CONTEXT((#3557))
GLOBAL_UNIT_ASSIGNED_CONTEXT((#3582,#3584,#3585))
REPRESENTATION_CONTEXT('','3D')
);
#3577=(
GEOMETRIC_REPRESENTATION_CONTEXT(3)
GLOBAL_UNCERTAINTY_ASSIGNED_CONTEXT((#3558))
GLOBAL_UNIT_ASSIGNED_CONTEXT((#3582,#3584,#3585))
REPRESENTATION_CONTEXT('','3D')
);
#3578=(
GEOMETRIC_REPRESENTATION_CONTEXT(3)
GLOBAL_UNCERTAINTY_ASSIGNED_CONTEXT((#3559))
GLOBAL_UNIT_ASSIGNED_CONTEXT((#3582,#3584,#3585))
REPRESENTATION_CONTEXT('','3D')
);
#3579=(
GEOMETRIC_REPRESENTATION_CONTEXT(3)
GLOBAL_UNCERTAINTY_ASSIGNED_CONTEXT((#3560))
GLOBAL_UNIT_ASSIGNED_CONTEXT((#3582,#3584,#3585))
REPRESENTATION_CONTEXT('','3D')
);
#3580=(
GEOMETRIC_REPRESENTATION_CONTEXT(3)
GLOBAL_UNCERTAINTY_ASSIGNED_CONTEXT((#3561))
GLOBAL_UNIT_ASSIGNED_CONTEXT((#3582,#3584,#3585))
REPRESENTATION_CONTEXT('','3D')
);
#3581=(
GEOMETRIC_REPRESENTATION_CONTEXT(3)
GLOBAL_UNCERTAINTY_ASSIGNED_CONTEXT((#3562))
GLOBAL_UNIT_ASSIGNED_CONTEXT((#3582,#3584,#3585))
REPRESENTATION_CONTEXT('','3D')
);
#3582=(
LENGTH_UNIT()
NAMED_UNIT(*)
SI_UNIT(.MILLI.,.METRE.)
);
#3583=(
LENGTH_UNIT()
NAMED_UNIT(*)
SI_UNIT($,.METRE.)
);
#3584=(
NAMED_UNIT(*)
PLANE_ANGLE_UNIT()
SI_UNIT($,.RADIAN.)
);
#3585=(
NAMED_UNIT(*)
SI_UNIT($,.STERADIAN.)
SOLID_ANGLE_UNIT()
);
#3586=SHAPE_DEFINITION_REPRESENTATION(#3604,#3681);
#3587=SHAPE_DEFINITION_REPRESENTATION(#3605,#3682);
#3588=SHAPE_DEFINITION_REPRESENTATION(#3606,#3683);
#3589=SHAPE_DEFINITION_REPRESENTATION(#3607,#3684);
#3590=SHAPE_DEFINITION_REPRESENTATION(#3608,#3685);
#3591=SHAPE_DEFINITION_REPRESENTATION(#3609,#3686);
#3592=SHAPE_DEFINITION_REPRESENTATION(#3610,#3687);
#3593=SHAPE_DEFINITION_REPRESENTATION(#3611,#3688);
#3594=SHAPE_DEFINITION_REPRESENTATION(#3612,#3689);
#3595=SHAPE_DEFINITION_REPRESENTATION(#3613,#3690);
#3596=SHAPE_DEFINITION_REPRESENTATION(#3614,#3691);
#3597=SHAPE_DEFINITION_REPRESENTATION(#3615,#3692);
#3598=SHAPE_DEFINITION_REPRESENTATION(#3616,#3693);
#3599=SHAPE_DEFINITION_REPRESENTATION(#3617,#3694);
#3600=SHAPE_DEFINITION_REPRESENTATION(#3618,#3695);
#3601=SHAPE_DEFINITION_REPRESENTATION(#3619,#3696);
#3602=SHAPE_DEFINITION_REPRESENTATION(#3620,#3697);
#3603=SHAPE_DEFINITION_REPRESENTATION(#3621,#3698);
#3604=PRODUCT_DEFINITION_SHAPE('',$,#3700);
#3605=PRODUCT_DEFINITION_SHAPE('',$,#3701);
#3606=PRODUCT_DEFINITION_SHAPE('',$,#3702);
#3607=PRODUCT_DEFINITION_SHAPE('',$,#3703);
#3608=PRODUCT_DEFINITION_SHAPE('',$,#3704);
#3609=PRODUCT_DEFINITION_SHAPE('',$,#3705);
#3610=PRODUCT_DEFINITION_SHAPE('',$,#3706);
#3611=PRODUCT_DEFINITION_SHAPE('',$,#3707);
#3612=PRODUCT_DEFINITION_SHAPE('',$,#3708);
#3613=PRODUCT_DEFINITION_SHAPE('',$,#3709);
#3614=PRODUCT_DEFINITION_SHAPE('',$,#3710);
#3615=PRODUCT_DEFINITION_SHAPE('',$,#3711);
#3616=PRODUCT_DEFINITION_SHAPE('',$,#3712);
#3617=PRODUCT_DEFINITION_SHAPE('',$,#3713);
#3618=PRODUCT_DEFINITION_SHAPE('',$,#3714);
#3619=PRODUCT_DEFINITION_SHAPE('',$,#3715);
#3620=PRODUCT_DEFINITION_SHAPE('',$,#3716);
#3621=PRODUCT_DEFINITION_SHAPE('',$,#3717);
#3622=PRODUCT_DEFINITION_SHAPE($,$,#188);
#3623=PRODUCT_DEFINITION_SHAPE($,$,#189);
#3624=PRODUCT_DEFINITION_SHAPE($,$,#190);
#3625=PRODUCT_DEFINITION_SHAPE($,$,#191);
#3626=PRODUCT_DEFINITION_SHAPE($,$,#192);
#3627=PRODUCT_DEFINITION_SHAPE($,$,#193);
#3628=PRODUCT_DEFINITION_SHAPE($,$,#194);
#3629=PRODUCT_DEFINITION_SHAPE($,$,#195);
#3630=PRODUCT_DEFINITION_SHAPE($,$,#196);
#3631=PRODUCT_DEFINITION_SHAPE($,$,#197);
#3632=PRODUCT_DEFINITION_SHAPE($,$,#198);
#3633=PRODUCT_DEFINITION_SHAPE($,$,#199);
#3634=PRODUCT_DEFINITION_SHAPE($,$,#200);
#3635=PRODUCT_DEFINITION_SHAPE($,$,#201);
#3636=PRODUCT_DEFINITION_SHAPE($,$,#202);
#3637=PRODUCT_DEFINITION_SHAPE($,$,#203);
#3638=PRODUCT_DEFINITION_SHAPE($,$,#204);
#3639=PRODUCT_DEFINITION_SHAPE($,$,#205);
#3640=PRODUCT_DEFINITION_SHAPE($,$,#206);
#3641=PRODUCT_DEFINITION_SHAPE($,$,#207);
#3642=PRODUCT_DEFINITION_SHAPE($,$,#208);
#3643=PRODUCT_DEFINITION_SHAPE($,$,#209);
#3644=PRODUCT_DEFINITION_SHAPE($,$,#210);
#3645=PRODUCT_DEFINITION_SHAPE($,$,#211);
#3646=PRODUCT_DEFINITION_SHAPE($,$,#212);
#3647=PRODUCT_DEFINITION_SHAPE($,$,#213);
#3648=PRODUCT_DEFINITION_SHAPE($,$,#214);
#3649=PRODUCT_DEFINITION_SHAPE($,$,#215);
#3650=PRODUCT_DEFINITION_SHAPE($,$,#216);
#3651=PRODUCT_DEFINITION_SHAPE($,$,#217);
#3652=PRODUCT_DEFINITION_SHAPE($,$,#218);
#3653=PRODUCT_DEFINITION_SHAPE($,$,#219);
#3654=PRODUCT_DEFINITION_SHAPE($,$,#220);
#3655=PRODUCT_DEFINITION_SHAPE($,$,#221);
#3656=PRODUCT_DEFINITION_SHAPE($,$,#222);
#3657=PRODUCT_DEFINITION_SHAPE($,$,#223);
#3658=PRODUCT_DEFINITION_SHAPE($,$,#224);
#3659=PRODUCT_DEFINITION_SHAPE($,$,#225);
#3660=PRODUCT_DEFINITION_SHAPE($,$,#226);
#3661=PRODUCT_DEFINITION_SHAPE($,$,#227);
#3662=PRODUCT_DEFINITION_SHAPE($,$,#228);
#3663=PRODUCT_DEFINITION_SHAPE($,$,#229);
#3664=PRODUCT_DEFINITION_SHAPE($,$,#230);
#3665=PRODUCT_DEFINITION_SHAPE($,$,#231);
#3666=PRODUCT_DEFINITION_SHAPE($,$,#232);
#3667=PRODUCT_DEFINITION_SHAPE($,$,#233);
#3668=PRODUCT_DEFINITION_SHAPE($,$,#234);
#3669=PRODUCT_DEFINITION_SHAPE($,$,#235);
#3670=PRODUCT_DEFINITION_SHAPE($,$,#236);
#3671=PRODUCT_DEFINITION_SHAPE($,$,#237);
#3672=PRODUCT_DEFINITION_SHAPE($,$,#238);
#3673=PRODUCT_DEFINITION_SHAPE($,$,#239);
#3674=PRODUCT_DEFINITION_SHAPE($,$,#240);
#3675=PRODUCT_DEFINITION_SHAPE($,$,#241);
#3676=PRODUCT_DEFINITION_SHAPE($,$,#242);
#3677=PRODUCT_DEFINITION_SHAPE($,$,#243);
#3678=PRODUCT_DEFINITION_SHAPE($,$,#244);
#3679=PRODUCT_DEFINITION_SHAPE($,$,#245);
#3680=PRODUCT_DEFINITION_SHAPE($,$,#246);
#3681=SHAPE_REPRESENTATION('',(#2073,#2300,#2301,#2302,#2303,#2304,#2305,
#2306,#2307,#2308,#2309,#2310,#2311,#2312,#2313,#2314,#2315,#2316,#2317,
#2318,#2319,#2320,#2321,#2322,#2323,#2324,#2325,#2326,#2327,#2328,#2329,
#2330,#2331,#2332,#2333,#2334,#2335,#2336,#2337,#2338,#2339,#2340,#2341,
#2342,#2343,#2344,#2345,#2346,#2347,#2348,#2349,#2350,#2351,#2352,#2353,
#2354,#2355,#2356,#2357,#2358),#3563);
#3682=SHAPE_REPRESENTATION('',(#2074),#3564);
#3683=SHAPE_REPRESENTATION('',(#2096),#3565);
#3684=SHAPE_REPRESENTATION('',(#2105),#3566);
#3685=SHAPE_REPRESENTATION('',(#2115),#3567);
#3686=SHAPE_REPRESENTATION('',(#2132),#3568);
#3687=SHAPE_REPRESENTATION('',(#2138),#3569);
#3688=SHAPE_REPRESENTATION('',(#2155),#3570);
#3689=SHAPE_REPRESENTATION('',(#2172),#3571);
#3690=SHAPE_REPRESENTATION('',(#2190),#3572);
#3691=SHAPE_REPRESENTATION('',(#2208),#3573);
#3692=SHAPE_REPRESENTATION('',(#2217),#3574);
#3693=SHAPE_REPRESENTATION('',(#2238),#3575);
#3694=SHAPE_REPRESENTATION('',(#2247),#3576);
#3695=SHAPE_REPRESENTATION('',(#2253),#3577);
#3696=SHAPE_REPRESENTATION('',(#2271),#3578);
#3697=SHAPE_REPRESENTATION('',(#2280),#3579);
#3698=SHAPE_REPRESENTATION('',(#2289),#3580);
#3699=PRODUCT_DEFINITION_CONTEXT('part definition',#3755,'design');
#3700=PRODUCT_DEFINITION('MAS-228','MAS-228',#3718,#3699);
#3701=PRODUCT_DEFINITION('Base plate','Base plate',#3719,#3699);
#3702=PRODUCT_DEFINITION('Pivot pedestal','Pivot pedestal',#3720,#3699);
#3703=PRODUCT_DEFINITION('Bearing bridge','Bearing bridge',#3721,#3699);
#3704=PRODUCT_DEFINITION('Driving crank','Driving crank',#3722,#3699);
#3705=PRODUCT_DEFINITION('Bridge column','Bridge column',#3723,#3699);
#3706=PRODUCT_DEFINITION('Radius arm','Radius arm',#3724,#3699);
#3707=PRODUCT_DEFINITION('Cell link','Cell link',#3725,#3699);
#3708=PRODUCT_DEFINITION('Ground pivot pin','Ground pivot pin',#3726,#3699);
#3709=PRODUCT_DEFINITION('Crank pivot pin','Crank pivot pin',#3727,#3699);
#3710=PRODUCT_DEFINITION('Crank spacer','Crank spacer',#3728,#3699);
#3711=PRODUCT_DEFINITION('Hollow cell pivot pin',
'Hollow cell pivot pin',#3729,#3699);
#3712=PRODUCT_DEFINITION('Pivot bushing','Pivot bushing',#3730,#3699);
#3713=PRODUCT_DEFINITION('Output stylus','Output stylus',#3731,#3699);
#3714=PRODUCT_DEFINITION('Cell pivot pin','Cell pivot pin',#3732,#3699);
#3715=PRODUCT_DEFINITION('Cell spacer','Cell spacer',#3733,#3699);
#3716=PRODUCT_DEFINITION('Pivot washer','Pivot washer',#3734,#3699);
#3717=PRODUCT_DEFINITION('Pivot retaining ring','Pivot retaining ring',
#3735,#3699);
#3718=PRODUCT_DEFINITION_FORMATION('',$,#3757);
#3719=PRODUCT_DEFINITION_FORMATION('',$,#3758);
#3720=PRODUCT_DEFINITION_FORMATION('',$,#3759);
#3721=PRODUCT_DEFINITION_FORMATION('',$,#3760);
#3722=PRODUCT_DEFINITION_FORMATION('',$,#3761);
#3723=PRODUCT_DEFINITION_FORMATION('',$,#3762);
#3724=PRODUCT_DEFINITION_FORMATION('',$,#3763);
#3725=PRODUCT_DEFINITION_FORMATION('',$,#3764);
#3726=PRODUCT_DEFINITION_FORMATION('',$,#3765);
#3727=PRODUCT_DEFINITION_FORMATION('',$,#3766);
#3728=PRODUCT_DEFINITION_FORMATION('',$,#3767);
#3729=PRODUCT_DEFINITION_FORMATION('',$,#3768);
#3730=PRODUCT_DEFINITION_FORMATION('',$,#3769);
#3731=PRODUCT_DEFINITION_FORMATION('',$,#3770);
#3732=PRODUCT_DEFINITION_FORMATION('',$,#3771);
#3733=PRODUCT_DEFINITION_FORMATION('',$,#3772);
#3734=PRODUCT_DEFINITION_FORMATION('',$,#3773);
#3735=PRODUCT_DEFINITION_FORMATION('',$,#3774);
#3736=PRODUCT_RELATED_PRODUCT_CATEGORY('MAS-228','MAS-228',(#3757));
#3737=PRODUCT_RELATED_PRODUCT_CATEGORY('Base plate','Base plate',(#3758));
#3738=PRODUCT_RELATED_PRODUCT_CATEGORY('Pivot pedestal',
'Pivot pedestal',(#3759));
#3739=PRODUCT_RELATED_PRODUCT_CATEGORY('Bearing bridge',
'Bearing bridge',(#3760));
#3740=PRODUCT_RELATED_PRODUCT_CATEGORY('Driving crank','Driving crank',
(#3761));
#3741=PRODUCT_RELATED_PRODUCT_CATEGORY('Bridge column','Bridge column',
(#3762));
#3742=PRODUCT_RELATED_PRODUCT_CATEGORY('Radius arm','Radius arm',(#3763));
#3743=PRODUCT_RELATED_PRODUCT_CATEGORY('Cell link','Cell link',(#3764));
#3744=PRODUCT_RELATED_PRODUCT_CATEGORY('Ground pivot pin',
'Ground pivot pin',(#3765));
#3745=PRODUCT_RELATED_PRODUCT_CATEGORY('Crank pivot pin',
'Crank pivot pin',(#3766));
#3746=PRODUCT_RELATED_PRODUCT_CATEGORY('Crank spacer','Crank spacer',(#3767));
#3747=PRODUCT_RELATED_PRODUCT_CATEGORY('Hollow cell pivot pin',
'Hollow cell pivot pin',(#3768));
#3748=PRODUCT_RELATED_PRODUCT_CATEGORY('Pivot bushing','Pivot bushing',
(#3769));
#3749=PRODUCT_RELATED_PRODUCT_CATEGORY('Output stylus','Output stylus',
(#3770));
#3750=PRODUCT_RELATED_PRODUCT_CATEGORY('Cell pivot pin',
'Cell pivot pin',(#3771));
#3751=PRODUCT_RELATED_PRODUCT_CATEGORY('Cell spacer','Cell spacer',(#3772));
#3752=PRODUCT_RELATED_PRODUCT_CATEGORY('Pivot washer','Pivot washer',(#3773));
#3753=PRODUCT_RELATED_PRODUCT_CATEGORY('Pivot retaining ring',
'Pivot retaining ring',(#3774));
#3754=APPLICATION_PROTOCOL_DEFINITION('international standard',
'automotive_design',2009,#3755);
#3755=APPLICATION_CONTEXT(
'Core Data for Automotive Mechanical Design Process');
#3756=PRODUCT_CONTEXT('part definition',#3755,'mechanical');
#3757=PRODUCT('MAS-228','MAS-228',
'Independent Peaucellier-Lipkin straight-line linkage. Radius arms 100
 mm, inversion-cell links 60 mm, crank radius and fixed-pivot spacing 
32 mm. Inversion constant 6400 mm squared, nominal output straight lin
e X=100 mm. Overhead bearing bridge clears the layered moving links. N
o accuracy or load rating assigned.',(#3756));
#3758=PRODUCT('Base plate','Base plate','Base plate',(#3756));
#3759=PRODUCT('Pivot pedestal','Pivot pedestal','Pivot pedestal',(#3756));
#3760=PRODUCT('Bearing bridge','Bearing bridge',$,(#3756));
#3761=PRODUCT('Driving crank','Driving crank','Driving crank',(#3756));
#3762=PRODUCT('Bridge column','Bridge column',$,(#3756));
#3763=PRODUCT('Radius arm','Radius arm',$,(#3756));
#3764=PRODUCT('Cell link','Cell link',$,(#3756));
#3765=PRODUCT('Ground pivot pin','Ground pivot pin',$,(#3756));
#3766=PRODUCT('Crank pivot pin','Crank pivot pin',$,(#3756));
#3767=PRODUCT('Crank spacer','Crank spacer','Crank spacer',(#3756));
#3768=PRODUCT('Hollow cell pivot pin','Hollow cell pivot pin',$,(#3756));
#3769=PRODUCT('Pivot bushing','Pivot bushing',$,(#3756));
#3770=PRODUCT('Output stylus','Output stylus',$,(#3756));
#3771=PRODUCT('Cell pivot pin','Cell pivot pin',$,(#3756));
#3772=PRODUCT('Cell spacer','Cell spacer',$,(#3756));
#3773=PRODUCT('Pivot washer','Pivot washer',$,(#3756));
#3774=PRODUCT('Pivot retaining ring','Pivot retaining ring',$,(#3756));
#3775=PRESENTATION_STYLE_ASSIGNMENT((#3788));
#3776=PRESENTATION_STYLE_ASSIGNMENT((#3789));
#3777=PRESENTATION_STYLE_ASSIGNMENT((#3790));
#3778=PRESENTATION_STYLE_ASSIGNMENT((#3791));
#3779=PRESENTATION_STYLE_ASSIGNMENT((#3792));
#3780=PRESENTATION_STYLE_ASSIGNMENT((#3793));
#3781=PRESENTATION_STYLE_ASSIGNMENT((#3794));
#3782=PRESENTATION_STYLE_ASSIGNMENT((#3795));
#3783=PRESENTATION_STYLE_ASSIGNMENT((#3796));
#3784=PRESENTATION_STYLE_ASSIGNMENT((#3797));
#3785=PRESENTATION_STYLE_ASSIGNMENT((#3798));
#3786=PRESENTATION_STYLE_ASSIGNMENT((#3799));
#3787=PRESENTATION_STYLE_ASSIGNMENT((#3800));
#3788=SURFACE_STYLE_USAGE(.BOTH.,#3801);
#3789=SURFACE_STYLE_USAGE(.BOTH.,#3802);
#3790=SURFACE_STYLE_USAGE(.BOTH.,#3803);
#3791=SURFACE_STYLE_USAGE(.BOTH.,#3804);
#3792=SURFACE_STYLE_USAGE(.BOTH.,#3805);
#3793=SURFACE_STYLE_USAGE(.BOTH.,#3806);
#3794=SURFACE_STYLE_USAGE(.BOTH.,#3807);
#3795=SURFACE_STYLE_USAGE(.BOTH.,#3808);
#3796=SURFACE_STYLE_USAGE(.BOTH.,#3809);
#3797=SURFACE_STYLE_USAGE(.BOTH.,#3810);
#3798=SURFACE_STYLE_USAGE(.BOTH.,#3811);
#3799=SURFACE_STYLE_USAGE(.BOTH.,#3812);
#3800=SURFACE_STYLE_USAGE(.BOTH.,#3813);
#3801=SURFACE_SIDE_STYLE('',(#3814));
#3802=SURFACE_SIDE_STYLE('',(#3815));
#3803=SURFACE_SIDE_STYLE('',(#3816));
#3804=SURFACE_SIDE_STYLE('',(#3817));
#3805=SURFACE_SIDE_STYLE('',(#3818));
#3806=SURFACE_SIDE_STYLE('',(#3819));
#3807=SURFACE_SIDE_STYLE('',(#3820));
#3808=SURFACE_SIDE_STYLE('',(#3821));
#3809=SURFACE_SIDE_STYLE('',(#3822));
#3810=SURFACE_SIDE_STYLE('',(#3823));
#3811=SURFACE_SIDE_STYLE('',(#3824));
#3812=SURFACE_SIDE_STYLE('',(#3825));
#3813=SURFACE_SIDE_STYLE('',(#3826));
#3814=SURFACE_STYLE_FILL_AREA(#3827);
#3815=SURFACE_STYLE_FILL_AREA(#3828);
#3816=SURFACE_STYLE_FILL_AREA(#3829);
#3817=SURFACE_STYLE_FILL_AREA(#3830);
#3818=SURFACE_STYLE_FILL_AREA(#3831);
#3819=SURFACE_STYLE_FILL_AREA(#3832);
#3820=SURFACE_STYLE_FILL_AREA(#3833);
#3821=SURFACE_STYLE_FILL_AREA(#3834);
#3822=SURFACE_STYLE_FILL_AREA(#3835);
#3823=SURFACE_STYLE_FILL_AREA(#3836);
#3824=SURFACE_STYLE_FILL_AREA(#3837);
#3825=SURFACE_STYLE_FILL_AREA(#3838);
#3826=SURFACE_STYLE_FILL_AREA(#3839);
#3827=FILL_AREA_STYLE('Steel - Satin',(#3840));
#3828=FILL_AREA_STYLE('Base gray',(#3841));
#3829=FILL_AREA_STYLE('Support gray',(#3842));
#3830=FILL_AREA_STYLE('Dark blue',(#3843));
#3831=FILL_AREA_STYLE('Driving crank finish',(#3844));
#3832=FILL_AREA_STYLE('Radius arm finish',(#3845));
#3833=FILL_AREA_STYLE('Cell link finish',(#3846));
#3834=FILL_AREA_STYLE('Pivot gray',(#3847));
#3835=FILL_AREA_STYLE('Spacer light gray',(#3848));
#3836=FILL_AREA_STYLE('Bearing light gray',(#3849));
#3837=FILL_AREA_STYLE('Stylus light gray',(#3850));
#3838=FILL_AREA_STYLE('Washer light gray',(#3851));
#3839=FILL_AREA_STYLE('Dark gray',(#3852));
#3840=FILL_AREA_STYLE_COLOUR('Steel - Satin',#3853);
#3841=FILL_AREA_STYLE_COLOUR('Base gray',#3854);
#3842=FILL_AREA_STYLE_COLOUR('Support gray',#3855);
#3843=FILL_AREA_STYLE_COLOUR('Dark blue',#3856);
#3844=FILL_AREA_STYLE_COLOUR('Driving crank finish',#3857);
#3845=FILL_AREA_STYLE_COLOUR('Radius arm finish',#3858);
#3846=FILL_AREA_STYLE_COLOUR('Cell link finish',#3859);
#3847=FILL_AREA_STYLE_COLOUR('Pivot gray',#3860);
#3848=FILL_AREA_STYLE_COLOUR('Spacer light gray',#3861);
#3849=FILL_AREA_STYLE_COLOUR('Bearing light gray',#3862);
#3850=FILL_AREA_STYLE_COLOUR('Stylus light gray',#3863);
#3851=FILL_AREA_STYLE_COLOUR('Washer light gray',#3864);
#3852=FILL_AREA_STYLE_COLOUR('Dark gray',#3865);
#3853=COLOUR_RGB('Steel - Satin',0.627450980392157,0.627450980392157,0.627450980392157);
#3854=COLOUR_RGB('Base gray',0.407843137254902,0.447058823529412,0.498039215686275);
#3855=COLOUR_RGB('Support gray',0.407843137254902,0.447058823529412,0.498039215686275);
#3856=COLOUR_RGB('Dark blue',0.0901960784313725,0.270588235294118,0.513725490196078);
#3857=COLOUR_RGB('Driving crank finish',0.662745098039216,0.831372549019608,
0.949019607843137);
#3858=COLOUR_RGB('Radius arm finish',0.0901960784313725,0.270588235294118,
0.513725490196078);
#3859=COLOUR_RGB('Cell link finish',0.317647058823529,0.686274509803922,
0.890196078431372);
#3860=COLOUR_RGB('Pivot gray',0.407843137254902,0.447058823529412,0.498039215686275);
#3861=COLOUR_RGB('Spacer light gray',0.725490196078431,0.752941176470588,
0.792156862745098);
#3862=COLOUR_RGB('Bearing light gray',0.725490196078431,0.752941176470588,
0.792156862745098);
#3863=COLOUR_RGB('Stylus light gray',0.725490196078431,0.752941176470588,
0.792156862745098);
#3864=COLOUR_RGB('Washer light gray',0.725490196078431,0.752941176470588,
0.792156862745098);
#3865=COLOUR_RGB('Dark gray',0.250980392156863,0.282352941176471,0.32156862745098);
ENDSEC;
END-ISO-10303-21;
